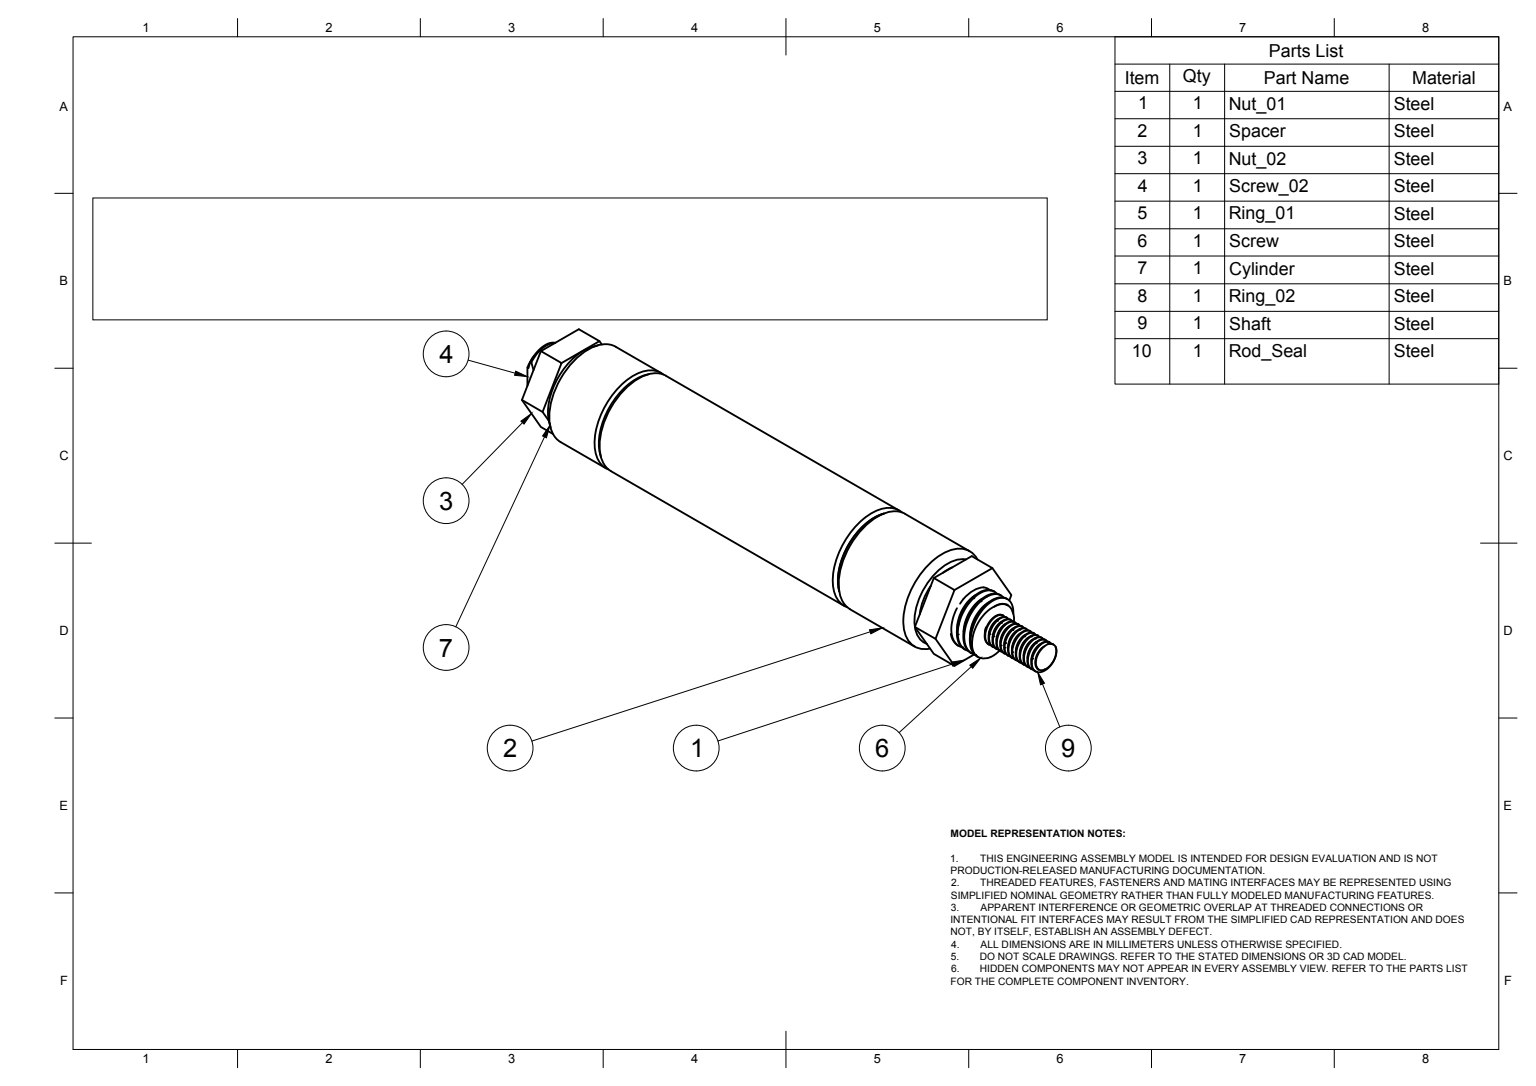
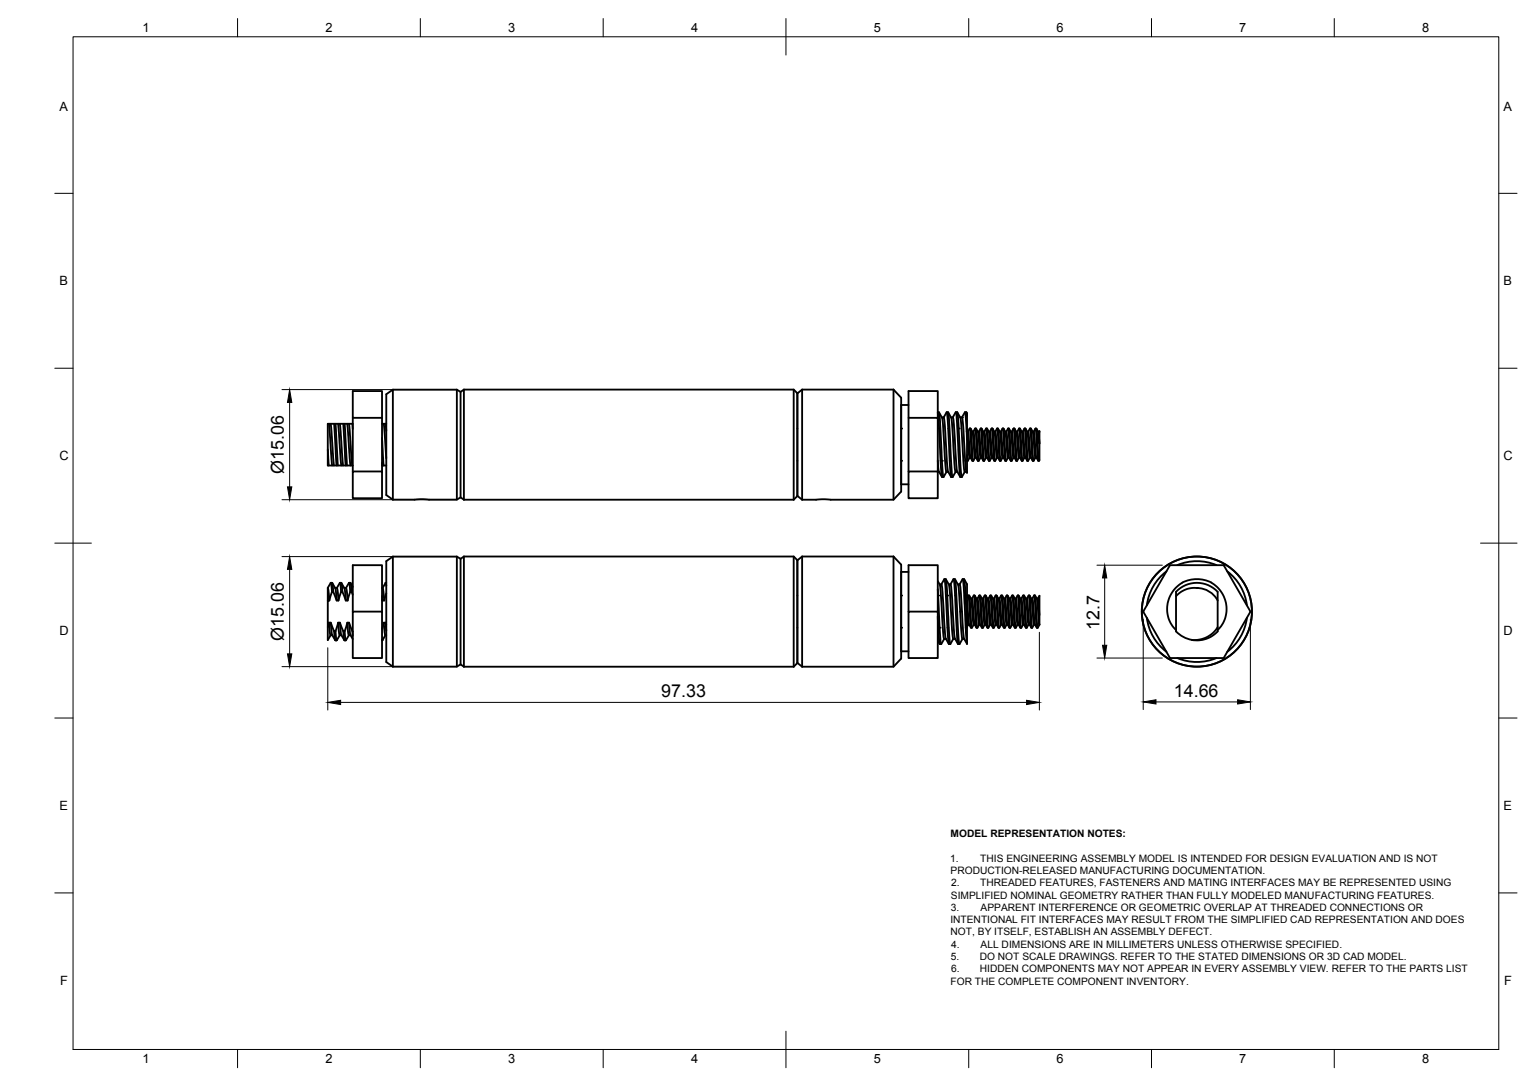
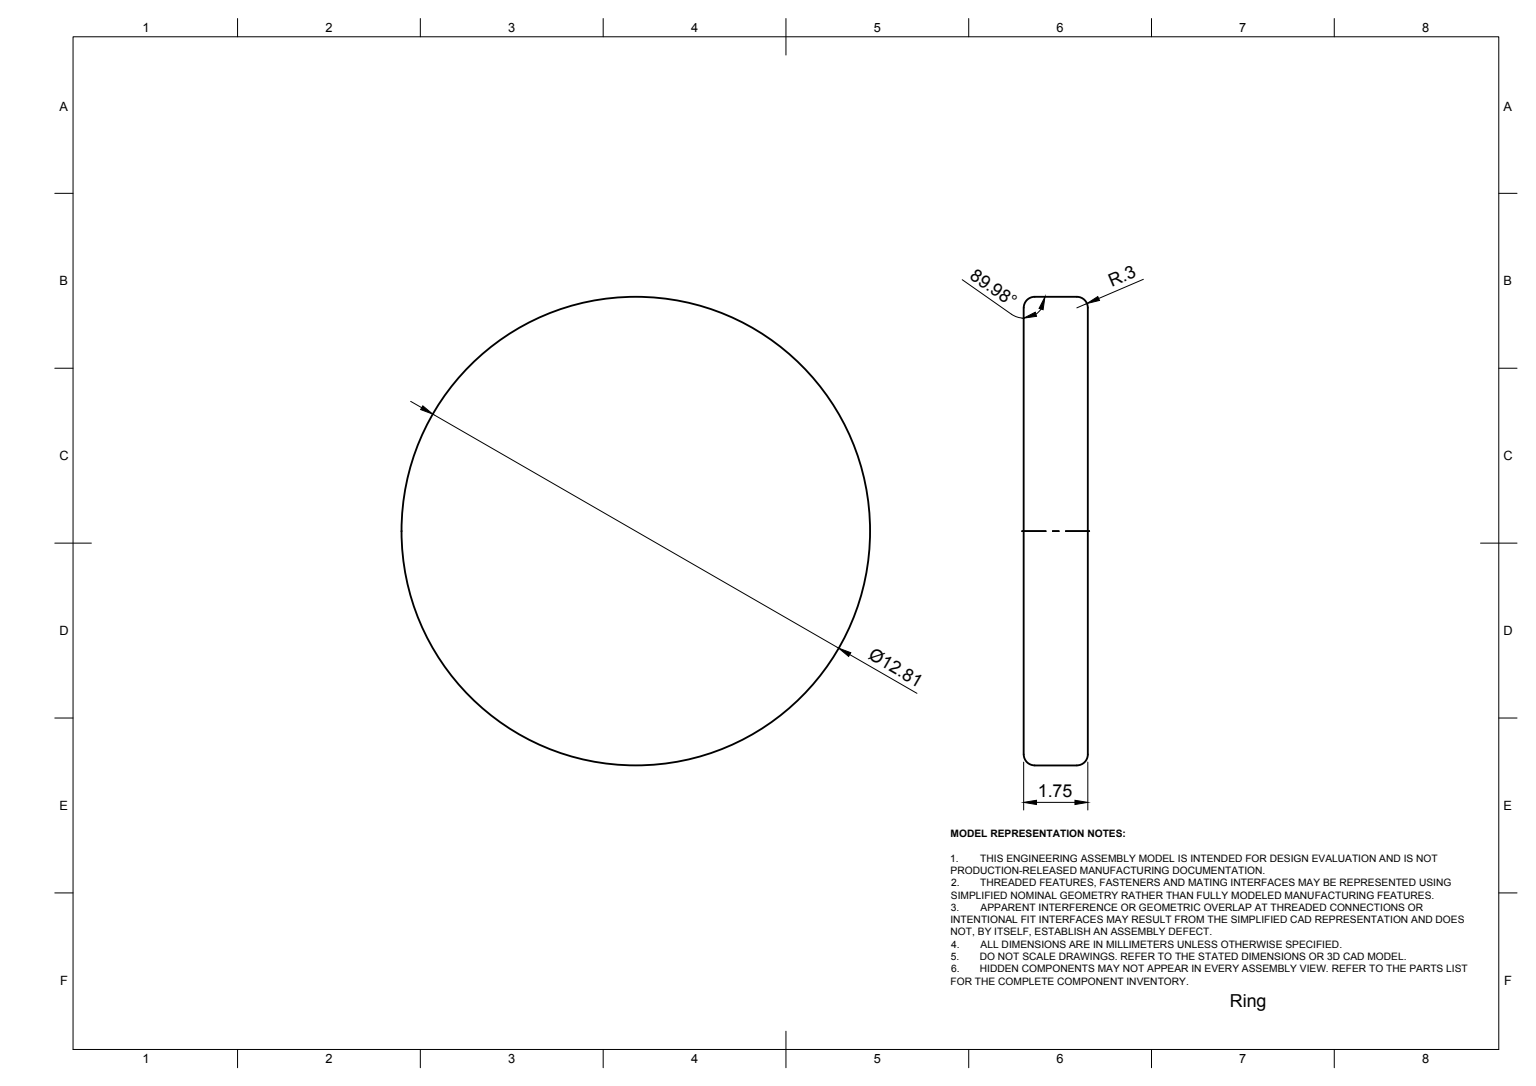
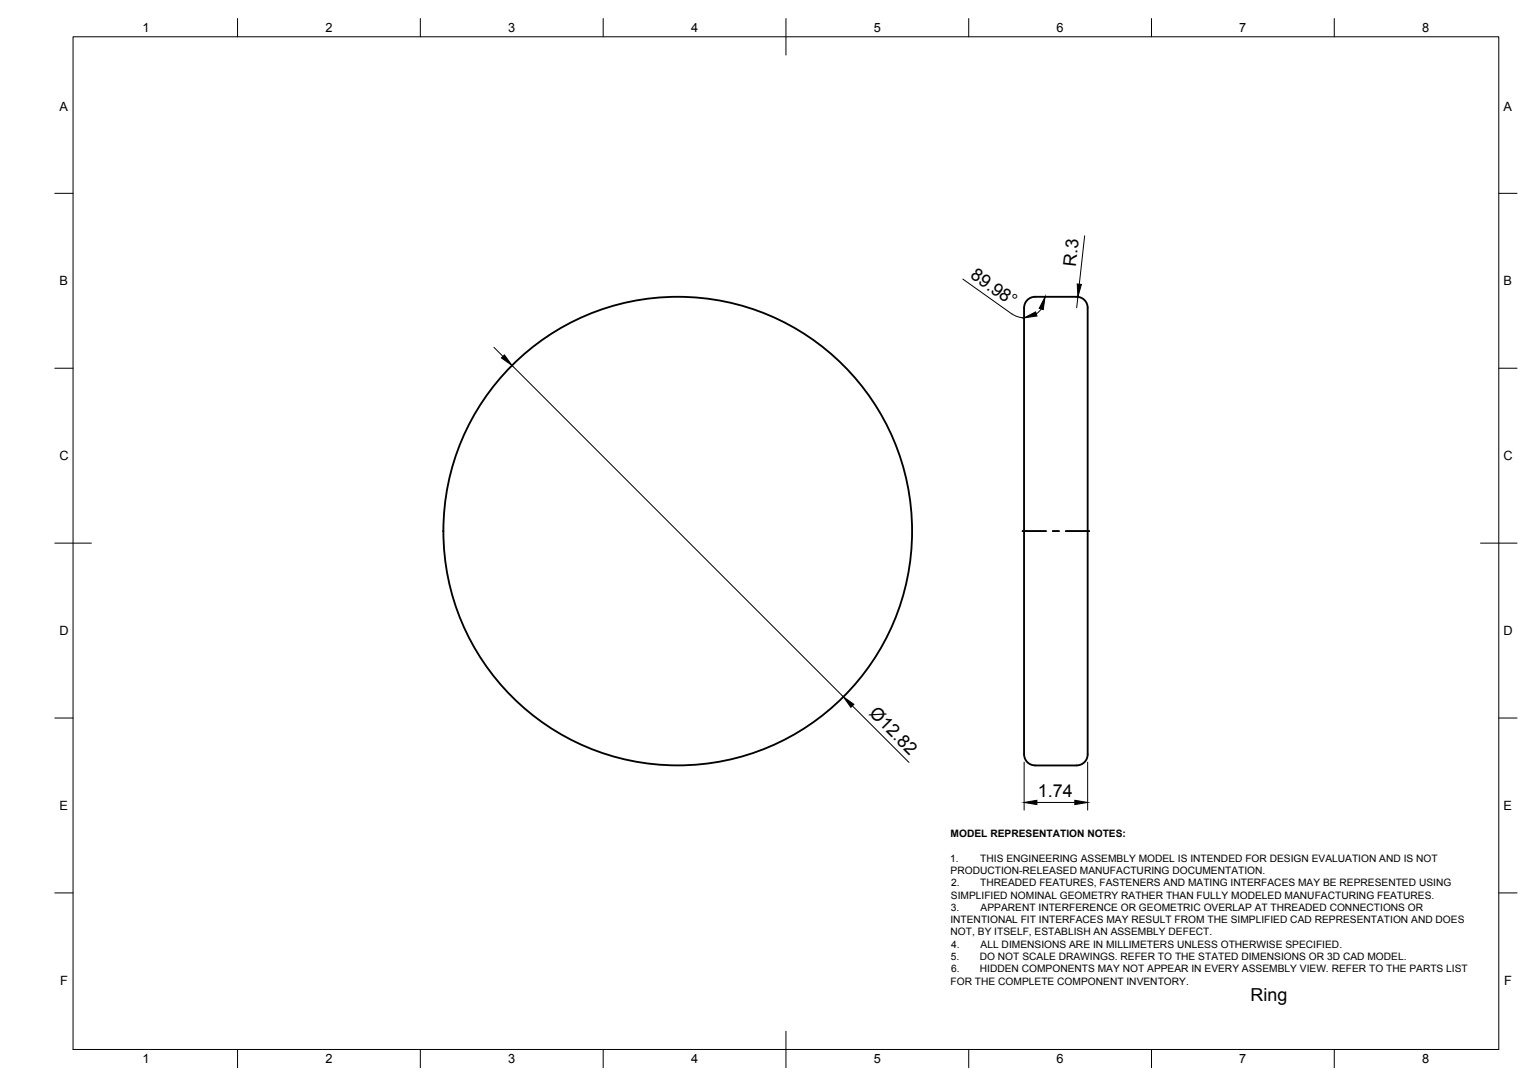
ISO-10303-21;
HEADER;
/* Generated by software containing ST-Developer
 * from STEP Tools, Inc. (www.steptools.com) 
 */

FILE_DESCRIPTION(
/* description */ (''),
/* implementation_level */ '2;1');

FILE_NAME(
/* name */ 'BR-314',
/* time_stamp */ '2026-10-06T13:15:55-07:00',
/* author */ (''),
/* organization */ (''),
/* preprocessor_version */ 'ST-DEVELOPER v20.2',
/* originating_system */ 'Autodesk Translation Framework v15.15.0.0',
/* authorisation */ '');

FILE_SCHEMA (('AUTOMOTIVE_DESIGN { 1 0 10303 214 3 1 1 }'));
ENDSEC;

DATA;
#10=MECHANICAL_DESIGN_GEOMETRIC_PRESENTATION_REPRESENTATION('',(#108,#109,
#110,#111,#112,#113,#114,#115,#116,#117),#27707);
#11=ITEM_DEFINED_TRANSFORMATION($,$,#3956,#4278);
#12=ITEM_DEFINED_TRANSFORMATION($,$,#3971,#4279);
#13=ITEM_DEFINED_TRANSFORMATION($,$,#3993,#4280);
#14=ITEM_DEFINED_TRANSFORMATION($,$,#4008,#4281);
#15=ITEM_DEFINED_TRANSFORMATION($,$,#4052,#4282);
#16=ITEM_DEFINED_TRANSFORMATION($,$,#4064,#4283);
#17=ITEM_DEFINED_TRANSFORMATION($,$,#4092,#4284);
#18=ITEM_DEFINED_TRANSFORMATION($,$,#4144,#4285);
#19=ITEM_DEFINED_TRANSFORMATION($,$,#4156,#4286);
#20=ITEM_DEFINED_TRANSFORMATION($,$,#4269,#4287);
#21=(
REPRESENTATION_RELATIONSHIP($,$,#27745,#27744)
REPRESENTATION_RELATIONSHIP_WITH_TRANSFORMATION(#11)
SHAPE_REPRESENTATION_RELATIONSHIP()
);
#22=(
REPRESENTATION_RELATIONSHIP($,$,#27746,#27744)
REPRESENTATION_RELATIONSHIP_WITH_TRANSFORMATION(#12)
SHAPE_REPRESENTATION_RELATIONSHIP()
);
#23=(
REPRESENTATION_RELATIONSHIP($,$,#27747,#27744)
REPRESENTATION_RELATIONSHIP_WITH_TRANSFORMATION(#13)
SHAPE_REPRESENTATION_RELATIONSHIP()
);
#24=(
REPRESENTATION_RELATIONSHIP($,$,#27748,#27744)
REPRESENTATION_RELATIONSHIP_WITH_TRANSFORMATION(#14)
SHAPE_REPRESENTATION_RELATIONSHIP()
);
#25=(
REPRESENTATION_RELATIONSHIP($,$,#27749,#27744)
REPRESENTATION_RELATIONSHIP_WITH_TRANSFORMATION(#15)
SHAPE_REPRESENTATION_RELATIONSHIP()
);
#26=(
REPRESENTATION_RELATIONSHIP($,$,#27750,#27744)
REPRESENTATION_RELATIONSHIP_WITH_TRANSFORMATION(#16)
SHAPE_REPRESENTATION_RELATIONSHIP()
);
#27=(
REPRESENTATION_RELATIONSHIP($,$,#27751,#27744)
REPRESENTATION_RELATIONSHIP_WITH_TRANSFORMATION(#17)
SHAPE_REPRESENTATION_RELATIONSHIP()
);
#28=(
REPRESENTATION_RELATIONSHIP($,$,#27752,#27744)
REPRESENTATION_RELATIONSHIP_WITH_TRANSFORMATION(#18)
SHAPE_REPRESENTATION_RELATIONSHIP()
);
#29=(
REPRESENTATION_RELATIONSHIP($,$,#27753,#27744)
REPRESENTATION_RELATIONSHIP_WITH_TRANSFORMATION(#19)
SHAPE_REPRESENTATION_RELATIONSHIP()
);
#30=(
REPRESENTATION_RELATIONSHIP($,$,#27754,#27744)
REPRESENTATION_RELATIONSHIP_WITH_TRANSFORMATION(#20)
SHAPE_REPRESENTATION_RELATIONSHIP()
);
#31=CONTEXT_DEPENDENT_SHAPE_REPRESENTATION(#21,#27734);
#32=CONTEXT_DEPENDENT_SHAPE_REPRESENTATION(#22,#27735);
#33=CONTEXT_DEPENDENT_SHAPE_REPRESENTATION(#23,#27736);
#34=CONTEXT_DEPENDENT_SHAPE_REPRESENTATION(#24,#27737);
#35=CONTEXT_DEPENDENT_SHAPE_REPRESENTATION(#25,#27738);
#36=CONTEXT_DEPENDENT_SHAPE_REPRESENTATION(#26,#27739);
#37=CONTEXT_DEPENDENT_SHAPE_REPRESENTATION(#27,#27740);
#38=CONTEXT_DEPENDENT_SHAPE_REPRESENTATION(#28,#27741);
#39=CONTEXT_DEPENDENT_SHAPE_REPRESENTATION(#29,#27742);
#40=CONTEXT_DEPENDENT_SHAPE_REPRESENTATION(#30,#27743);
#41=NEXT_ASSEMBLY_USAGE_OCCURRENCE('Nut_01:1','Nut_01:1','Nut_01:1',#27756,
#27757,'Nut_01:1');
#42=NEXT_ASSEMBLY_USAGE_OCCURRENCE('Spacer:1','Spacer:1','Spacer:1',#27756,
#27758,'Spacer:1');
#43=NEXT_ASSEMBLY_USAGE_OCCURRENCE('Nut_02:1','Nut_02:1','Nut_02:1',#27756,
#27759,'Nut_02:1');
#44=NEXT_ASSEMBLY_USAGE_OCCURRENCE('Screw_02:1','Screw_02:1',
'Screw_02:1',#27756,#27760,'Screw_02:1');
#45=NEXT_ASSEMBLY_USAGE_OCCURRENCE('Ring_01:1','Ring_01:1','Ring_01:1',
#27756,#27761,'Ring_01:1');
#46=NEXT_ASSEMBLY_USAGE_OCCURRENCE('Screw:1','Screw:1','Screw:1',#27756,
#27762,'Screw:1');
#47=NEXT_ASSEMBLY_USAGE_OCCURRENCE('Cylinder:1','Cylinder:1',
'Cylinder:1',#27756,#27763,'Cylinder:1');
#48=NEXT_ASSEMBLY_USAGE_OCCURRENCE('Ring_02:1','Ring_02:1','Ring_02:1',
#27756,#27764,'Ring_02:1');
#49=NEXT_ASSEMBLY_USAGE_OCCURRENCE('Shaft:1','Shaft:1','Shaft:1',#27756,
#27765,'Shaft:1');
#50=NEXT_ASSEMBLY_USAGE_OCCURRENCE('Rod_Seal:1','Rod_Seal:1',
'Rod_Seal:1',#27756,#27766,'Rod_Seal:1');
#51=TOROIDAL_SURFACE('',#4053,6.1074958342087,0.3);
#52=TOROIDAL_SURFACE('',#4060,6.1071549018742,0.3);
#53=TOROIDAL_SURFACE('',#4145,6.10923539706593,0.3);
#54=TOROIDAL_SURFACE('',#4152,6.1088989677085,0.3);
#55=TOROIDAL_SURFACE('',#4197,6.10845002480549,0.3);
#56=TOROIDAL_SURFACE('',#4203,6.107959450045,0.3);
#57=TOROIDAL_SURFACE('',#4209,4.18902817623056,0.3);
#58=TOROIDAL_SURFACE('',#4216,6.1096023907077,0.3);
#59=TOROIDAL_SURFACE('',#4223,6.10941276264524,0.3);
#60=TOROIDAL_SURFACE('',#4228,6.1087216021292,0.3);
#61=TOROIDAL_SURFACE('',#4236,6.1086273903848,0.3);
#62=TOROIDAL_SURFACE('',#4238,6.10778208446569,0.3);
#63=TOROIDAL_SURFACE('',#4243,6.10767319978801,0.3);
#64=TOROIDAL_SURFACE('',#4248,6.1069775362949,0.3);
#65=TOROIDAL_SURFACE('',#4256,6.10683442041659,0.3);
#66=TOROIDAL_SURFACE('',#4261,4.12329516333974,0.3);
#67=ELLIPSE('',#4027,3.36109563026061,2.90329889035631);
#68=ELLIPSE('',#4028,2.84121050972126,2.43735261139454);
#69=ELLIPSE('',#4046,3.33206993022602,2.82346550068506);
#70=CONICAL_SURFACE('',#3978,7.269,0.680431320864525);
#71=CONICAL_SURFACE('',#3982,6.974,0.81226843236958);
#72=CONICAL_SURFACE('',#4057,6.40732538114918,0.000295609290232334);
#73=CONICAL_SURFACE('',#4093,7.27835105742136,0.785398163397451);
#74=CONICAL_SURFACE('',#4106,7.20746054905241,0.610790367386849);
#75=CONICAL_SURFACE('',#4111,7.36529369971832,0.557210682142491);
#76=CONICAL_SURFACE('',#4113,7.36790580323689,0.610790367386849);
#77=CONICAL_SURFACE('',#4114,6.41628586403442,0.000295609290232646);
#78=CONICAL_SURFACE('',#4118,6.40906719549494,0.00029560929023293);
#79=CONICAL_SURFACE('',#4126,6.40820475053297,0.000295609290233083);
#80=CONICAL_SURFACE('',#4130,6.40732538114918,0.000295609290232334);
#81=CONICAL_SURFACE('',#4134,6.40667124022599,0.000295609290231853);
#82=CONICAL_SURFACE('',#4149,6.40906719549494,0.00029560929023293);
#83=CONICAL_SURFACE('',#4201,6.40820475053297,0.000295609290233083);
#84=CONICAL_SURFACE('',#4220,6.40950758978419,0.000295609290232241);
#85=CONICAL_SURFACE('',#4232,6.40867450936473,0.000295609290232273);
#86=CONICAL_SURFACE('',#4241,6.40772765523458,0.000295609290232245);
#87=CONICAL_SURFACE('',#4252,6.40690599146347,0.000295609290233429);
#88=SHAPE_REPRESENTATION_RELATIONSHIP('SRR','None',#27745,#98);
#89=SHAPE_REPRESENTATION_RELATIONSHIP('SRR','None',#27746,#99);
#90=SHAPE_REPRESENTATION_RELATIONSHIP('SRR','None',#27747,#100);
#91=SHAPE_REPRESENTATION_RELATIONSHIP('SRR','None',#27748,#101);
#92=SHAPE_REPRESENTATION_RELATIONSHIP('SRR','None',#27749,#102);
#93=SHAPE_REPRESENTATION_RELATIONSHIP('SRR','None',#27750,#103);
#94=SHAPE_REPRESENTATION_RELATIONSHIP('SRR','None',#27751,#104);
#95=SHAPE_REPRESENTATION_RELATIONSHIP('SRR','None',#27752,#105);
#96=SHAPE_REPRESENTATION_RELATIONSHIP('SRR','None',#27753,#106);
#97=SHAPE_REPRESENTATION_RELATIONSHIP('SRR','None',#27754,#107);
#98=ADVANCED_BREP_SHAPE_REPRESENTATION('',(#118),#27697);
#99=ADVANCED_BREP_SHAPE_REPRESENTATION('',(#119),#27698);
#100=ADVANCED_BREP_SHAPE_REPRESENTATION('',(#120),#27699);
#101=ADVANCED_BREP_SHAPE_REPRESENTATION('',(#121),#27700);
#102=ADVANCED_BREP_SHAPE_REPRESENTATION('',(#122),#27701);
#103=ADVANCED_BREP_SHAPE_REPRESENTATION('',(#123),#27702);
#104=ADVANCED_BREP_SHAPE_REPRESENTATION('',(#124),#27703);
#105=ADVANCED_BREP_SHAPE_REPRESENTATION('',(#125),#27704);
#106=ADVANCED_BREP_SHAPE_REPRESENTATION('',(#126),#27705);
#107=ADVANCED_BREP_SHAPE_REPRESENTATION('',(#127),#27706);
#108=STYLED_ITEM('',(#27804),#118);
#109=STYLED_ITEM('',(#27804),#119);
#110=STYLED_ITEM('',(#27804),#120);
#111=STYLED_ITEM('',(#27804),#121);
#112=STYLED_ITEM('',(#27804),#122);
#113=STYLED_ITEM('',(#27804),#123);
#114=STYLED_ITEM('',(#27804),#124);
#115=STYLED_ITEM('',(#27804),#125);
#116=STYLED_ITEM('',(#27804),#126);
#117=STYLED_ITEM('',(#27804),#127);
#118=MANIFOLD_SOLID_BREP('Body1',#3834);
#119=MANIFOLD_SOLID_BREP('Body1',#3835);
#120=MANIFOLD_SOLID_BREP('Body1',#3836);
#121=MANIFOLD_SOLID_BREP('Body1',#3837);
#122=MANIFOLD_SOLID_BREP('Body1',#3838);
#123=MANIFOLD_SOLID_BREP('Body1',#3839);
#124=MANIFOLD_SOLID_BREP('Body1',#3840);
#125=MANIFOLD_SOLID_BREP('Body1',#3841);
#126=MANIFOLD_SOLID_BREP('Body1',#3842);
#127=MANIFOLD_SOLID_BREP('Body1',#3843);
#128=FACE_BOUND('',#670,.T.);
#129=FACE_BOUND('',#672,.T.);
#130=FACE_BOUND('',#675,.T.);
#131=FACE_BOUND('',#677,.T.);
#132=FACE_BOUND('',#680,.T.);
#133=FACE_BOUND('',#683,.T.);
#134=FACE_BOUND('',#686,.T.);
#135=FACE_BOUND('',#689,.T.);
#136=FACE_BOUND('',#701,.T.);
#137=FACE_BOUND('',#703,.T.);
#138=FACE_BOUND('',#765,.T.);
#139=FACE_BOUND('',#789,.T.);
#140=FACE_BOUND('',#791,.T.);
#141=FACE_BOUND('',#793,.T.);
#142=FACE_BOUND('',#796,.T.);
#143=FACE_BOUND('',#801,.T.);
#144=FACE_BOUND('',#804,.T.);
#145=FACE_BOUND('',#811,.T.);
#146=FACE_BOUND('',#814,.T.);
#147=FACE_BOUND('',#821,.T.);
#148=FACE_BOUND('',#824,.T.);
#149=FACE_BOUND('',#826,.T.);
#150=FACE_BOUND('',#828,.T.);
#151=FACE_BOUND('',#835,.T.);
#152=FACE_BOUND('',#866,.T.);
#153=FACE_BOUND('',#871,.T.);
#154=FACE_BOUND('',#879,.T.);
#155=FACE_BOUND('',#883,.T.);
#156=FACE_BOUND('',#886,.T.);
#157=FACE_BOUND('',#890,.T.);
#158=FACE_BOUND('',#896,.T.);
#159=FACE_BOUND('',#900,.T.);
#160=FACE_BOUND('',#903,.T.);
#161=FACE_BOUND('',#911,.T.);
#162=FACE_BOUND('',#914,.T.);
#163=PLANE('',#3963);
#164=PLANE('',#3964);
#165=PLANE('',#3965);
#166=PLANE('',#3966);
#167=PLANE('',#3967);
#168=PLANE('',#3968);
#169=PLANE('',#3969);
#170=PLANE('',#3970);
#171=PLANE('',#3976);
#172=PLANE('',#3984);
#173=PLANE('',#3988);
#174=PLANE('',#3992);
#175=PLANE('',#4000);
#176=PLANE('',#4001);
#177=PLANE('',#4002);
#178=PLANE('',#4003);
#179=PLANE('',#4004);
#180=PLANE('',#4005);
#181=PLANE('',#4006);
#182=PLANE('',#4007);
#183=PLANE('',#4009);
#184=PLANE('',#4010);
#185=PLANE('',#4029);
#186=PLANE('',#4050);
#187=PLANE('',#4051);
#188=PLANE('',#4059);
#189=PLANE('',#4063);
#190=PLANE('',#4080);
#191=PLANE('',#4089);
#192=PLANE('',#4090);
#193=PLANE('',#4091);
#194=PLANE('',#4096);
#195=PLANE('',#4104);
#196=PLANE('',#4120);
#197=PLANE('',#4124);
#198=PLANE('',#4136);
#199=PLANE('',#4140);
#200=PLANE('',#4143);
#201=PLANE('',#4151);
#202=PLANE('',#4155);
#203=PLANE('',#4191);
#204=PLANE('',#4194);
#205=PLANE('',#4205);
#206=PLANE('',#4207);
#207=PLANE('',#4208);
#208=PLANE('',#4215);
#209=PLANE('',#4222);
#210=PLANE('',#4226);
#211=PLANE('',#4234);
#212=PLANE('',#4246);
#213=PLANE('',#4254);
#214=PLANE('',#4259);
#215=PLANE('',#4265);
#216=PLANE('',#4273);
#217=PLANE('',#4277);
#218=CIRCLE('',#3958,4.433);
#219=CIRCLE('',#3959,4.433);
#220=CIRCLE('',#3961,3.72275);
#221=CIRCLE('',#3962,3.72275);
#222=CIRCLE('',#3974,4.75);
#223=CIRCLE('',#3975,4.75);
#224=CIRCLE('',#3977,7.01);
#225=CIRCLE('',#3979,7.528);
#226=CIRCLE('',#3981,7.528);
#227=CIRCLE('',#3983,6.42);
#228=CIRCLE('',#3985,3.7);
#229=CIRCLE('',#3987,3.7);
#230=CIRCLE('',#3989,2.204);
#231=CIRCLE('',#3991,2.204);
#232=CIRCLE('',#3995,4.433);
#233=CIRCLE('',#3996,4.433);
#234=CIRCLE('',#3998,3.72275);
#235=CIRCLE('',#3999,3.72275);
#236=CIRCLE('',#4012,3.22275);
#237=CIRCLE('',#4026,3.22275);
#238=CIRCLE('',#4030,3.933);
#239=CIRCLE('',#4033,3.933);
#240=CIRCLE('',#4048,5.);
#241=CIRCLE('',#4049,5.);
#242=CIRCLE('',#4054,6.1074958342087);
#243=CIRCLE('',#4055,0.3);
#244=CIRCLE('',#4056,6.40749582110097);
#245=CIRCLE('',#4058,6.40715488876647);
#246=CIRCLE('',#4061,0.3);
#247=CIRCLE('',#4062,6.1071549018742);
#248=CIRCLE('',#4066,3.72275);
#249=CIRCLE('',#4073,3.72275);
#250=CIRCLE('',#4075,4.433);
#251=CIRCLE('',#4076,4.433);
#252=CIRCLE('',#4078,1.77625);
#253=CIRCLE('',#4079,1.77625);
#254=CIRCLE('',#4081,2.204);
#255=CIRCLE('',#4082,2.204);
#256=CIRCLE('',#4084,2.204);
#257=CIRCLE('',#4085,2.204);
#258=CIRCLE('',#4087,5.42440960677665);
#259=CIRCLE('',#4088,5.42440960677665);
#260=CIRCLE('',#4094,7.52835105742136);
#261=CIRCLE('',#4095,7.02835105742136);
#262=CIRCLE('',#4097,6.42021067919505);
#263=CIRCLE('',#4099,7.52835105742136);
#264=CIRCLE('',#4102,5.);
#265=CIRCLE('',#4103,5.);
#266=CIRCLE('',#4105,3.44589712386029);
#267=CIRCLE('',#4107,7.52312685038423);
#268=CIRCLE('',#4108,6.89179424772059);
#269=CIRCLE('',#4110,7.52312685038423);
#270=CIRCLE('',#4112,7.20746054905241);
#271=CIRCLE('',#4115,6.40969108660508);
#272=CIRCLE('',#4117,6.40969108660508);
#273=CIRCLE('',#4119,6.40881029802658);
#274=CIRCLE('',#4121,6.41550316824698);
#275=CIRCLE('',#4123,6.41550316824698);
#276=CIRCLE('',#4125,6.40853872070288);
#277=CIRCLE('',#4127,6.40787078036307);
#278=CIRCLE('',#4129,6.40787078036307);
#279=CIRCLE('',#4131,6.40706623219228);
#280=CIRCLE('',#4133,6.40706623219228);
#281=CIRCLE('',#4135,6.4065967297173);
#282=CIRCLE('',#4137,4.66385643997278);
#283=CIRCLE('',#4139,4.66385643997278);
#284=CIRCLE('',#4141,3.44589712386029);
#285=CIRCLE('',#4146,6.10923539706593);
#286=CIRCLE('',#4147,0.3);
#287=CIRCLE('',#4148,6.4092353839582);
#288=CIRCLE('',#4150,6.40889895460077);
#289=CIRCLE('',#4153,0.3);
#290=CIRCLE('',#4154,6.1088989677085);
#291=CIRCLE('',#4158,2.204);
#292=CIRCLE('',#4159,2.204);
#293=CIRCLE('',#4160,2.204);
#294=CIRCLE('',#4174,1.77625);
#295=CIRCLE('',#4188,1.77625);
#296=CIRCLE('',#4190,0.999999999999996);
#297=CIRCLE('',#4193,2.204);
#298=CIRCLE('',#4195,6.107959450045);
#299=CIRCLE('',#4196,6.10778208446569);
#300=CIRCLE('',#4198,6.10845002480549);
#301=CIRCLE('',#4199,0.3);
#302=CIRCLE('',#4200,6.40845001169777);
#303=CIRCLE('',#4202,6.40795943693727);
#304=CIRCLE('',#4204,0.3);
#305=CIRCLE('',#4206,6.1086273903848);
#306=CIRCLE('',#4210,4.18902817623056);
#307=CIRCLE('',#4211,0.3);
#308=CIRCLE('',#4212,4.48902817623056);
#309=CIRCLE('',#4214,4.48902817623056);
#310=CIRCLE('',#4217,6.1096023907077);
#311=CIRCLE('',#4218,0.3);
#312=CIRCLE('',#4219,6.40960237759997);
#313=CIRCLE('',#4221,6.40941274953751);
#314=CIRCLE('',#4224,0.3);
#315=CIRCLE('',#4225,6.10941276264524);
#316=CIRCLE('',#4227,2.21164758166987);
#317=CIRCLE('',#4229,6.1087216021292);
#318=CIRCLE('',#4230,0.3);
#319=CIRCLE('',#4231,6.40872158902147);
#320=CIRCLE('',#4233,6.40862737727707);
#321=CIRCLE('',#4235,2.21164758166987);
#322=CIRCLE('',#4237,0.3);
#323=CIRCLE('',#4239,0.3);
#324=CIRCLE('',#4240,6.40778207135796);
#325=CIRCLE('',#4242,6.40767318668028);
#326=CIRCLE('',#4244,0.3);
#327=CIRCLE('',#4245,6.10767319978801);
#328=CIRCLE('',#4247,2.21164758166987);
#329=CIRCLE('',#4249,6.1069775362949);
#330=CIRCLE('',#4250,0.3);
#331=CIRCLE('',#4251,6.40697752318717);
#332=CIRCLE('',#4253,6.40683440730886);
#333=CIRCLE('',#4255,2.21164758166987);
#334=CIRCLE('',#4257,0.3);
#335=CIRCLE('',#4258,6.10683442041659);
#336=CIRCLE('',#4260,4.42329516333974);
#337=CIRCLE('',#4262,4.42329516333974);
#338=CIRCLE('',#4263,0.3);
#339=CIRCLE('',#4264,4.12329516333974);
#340=CIRCLE('',#4271,3.7);
#341=CIRCLE('',#4272,3.7);
#342=CIRCLE('',#4274,2.204);
#343=CIRCLE('',#4276,2.204);
#344=CYLINDRICAL_SURFACE('',#3957,4.433);
#345=CYLINDRICAL_SURFACE('',#3960,3.72275);
#346=CYLINDRICAL_SURFACE('',#3972,0.999999999999996);
#347=CYLINDRICAL_SURFACE('',#3973,4.75);
#348=CYLINDRICAL_SURFACE('',#3980,7.528);
#349=CYLINDRICAL_SURFACE('',#3986,3.7);
#350=CYLINDRICAL_SURFACE('',#3990,2.204);
#351=CYLINDRICAL_SURFACE('',#3994,4.433);
#352=CYLINDRICAL_SURFACE('',#3997,3.72275);
#353=CYLINDRICAL_SURFACE('',#4011,3.22275);
#354=CYLINDRICAL_SURFACE('',#4013,3.22275);
#355=CYLINDRICAL_SURFACE('',#4014,3.22275);
#356=CYLINDRICAL_SURFACE('',#4015,3.22275);
#357=CYLINDRICAL_SURFACE('',#4016,3.22275);
#358=CYLINDRICAL_SURFACE('',#4017,3.22275);
#359=CYLINDRICAL_SURFACE('',#4018,3.22275);
#360=CYLINDRICAL_SURFACE('',#4019,3.22275);
#361=CYLINDRICAL_SURFACE('',#4020,3.22275);
#362=CYLINDRICAL_SURFACE('',#4021,3.22275);
#363=CYLINDRICAL_SURFACE('',#4022,3.22275);
#364=CYLINDRICAL_SURFACE('',#4023,3.22275);
#365=CYLINDRICAL_SURFACE('',#4024,3.22275);
#366=CYLINDRICAL_SURFACE('',#4025,3.22275);
#367=CYLINDRICAL_SURFACE('',#4031,3.933);
#368=CYLINDRICAL_SURFACE('',#4032,3.933);
#369=CYLINDRICAL_SURFACE('',#4034,3.933);
#370=CYLINDRICAL_SURFACE('',#4035,3.933);
#371=CYLINDRICAL_SURFACE('',#4036,3.933);
#372=CYLINDRICAL_SURFACE('',#4037,3.933);
#373=CYLINDRICAL_SURFACE('',#4038,3.933);
#374=CYLINDRICAL_SURFACE('',#4039,3.933);
#375=CYLINDRICAL_SURFACE('',#4040,3.933);
#376=CYLINDRICAL_SURFACE('',#4041,3.933);
#377=CYLINDRICAL_SURFACE('',#4042,3.933);
#378=CYLINDRICAL_SURFACE('',#4043,3.933);
#379=CYLINDRICAL_SURFACE('',#4044,3.933);
#380=CYLINDRICAL_SURFACE('',#4045,3.933);
#381=CYLINDRICAL_SURFACE('',#4047,5.);
#382=CYLINDRICAL_SURFACE('',#4065,3.72275);
#383=CYLINDRICAL_SURFACE('',#4067,3.72275);
#384=CYLINDRICAL_SURFACE('',#4068,3.72275);
#385=CYLINDRICAL_SURFACE('',#4069,3.72275);
#386=CYLINDRICAL_SURFACE('',#4070,3.72275);
#387=CYLINDRICAL_SURFACE('',#4071,3.72275);
#388=CYLINDRICAL_SURFACE('',#4072,3.72275);
#389=CYLINDRICAL_SURFACE('',#4074,4.433);
#390=CYLINDRICAL_SURFACE('',#4077,1.77625);
#391=CYLINDRICAL_SURFACE('',#4083,2.204);
#392=CYLINDRICAL_SURFACE('',#4086,5.42440960677665);
#393=CYLINDRICAL_SURFACE('',#4098,7.52835105742136);
#394=CYLINDRICAL_SURFACE('',#4100,0.999999999999999);
#395=CYLINDRICAL_SURFACE('',#4101,5.);
#396=CYLINDRICAL_SURFACE('',#4109,7.52312685038423);
#397=CYLINDRICAL_SURFACE('',#4116,6.40969108660508);
#398=CYLINDRICAL_SURFACE('',#4122,6.41550316824698);
#399=CYLINDRICAL_SURFACE('',#4128,6.40787078036307);
#400=CYLINDRICAL_SURFACE('',#4132,6.40706623219228);
#401=CYLINDRICAL_SURFACE('',#4138,4.66385643997278);
#402=CYLINDRICAL_SURFACE('',#4142,3.44589712386029);
#403=CYLINDRICAL_SURFACE('',#4157,2.204);
#404=CYLINDRICAL_SURFACE('',#4161,2.204);
#405=CYLINDRICAL_SURFACE('',#4162,2.204);
#406=CYLINDRICAL_SURFACE('',#4163,2.204);
#407=CYLINDRICAL_SURFACE('',#4164,2.204);
#408=CYLINDRICAL_SURFACE('',#4165,2.204);
#409=CYLINDRICAL_SURFACE('',#4166,2.204);
#410=CYLINDRICAL_SURFACE('',#4167,2.204);
#411=CYLINDRICAL_SURFACE('',#4168,2.204);
#412=CYLINDRICAL_SURFACE('',#4169,2.204);
#413=CYLINDRICAL_SURFACE('',#4170,2.204);
#414=CYLINDRICAL_SURFACE('',#4171,2.204);
#415=CYLINDRICAL_SURFACE('',#4172,2.204);
#416=CYLINDRICAL_SURFACE('',#4173,1.77625);
#417=CYLINDRICAL_SURFACE('',#4175,1.77625);
#418=CYLINDRICAL_SURFACE('',#4176,1.77625);
#419=CYLINDRICAL_SURFACE('',#4177,1.77625);
#420=CYLINDRICAL_SURFACE('',#4178,1.77625);
#421=CYLINDRICAL_SURFACE('',#4179,1.77625);
#422=CYLINDRICAL_SURFACE('',#4180,1.77625);
#423=CYLINDRICAL_SURFACE('',#4181,1.77625);
#424=CYLINDRICAL_SURFACE('',#4182,1.77625);
#425=CYLINDRICAL_SURFACE('',#4183,1.77625);
#426=CYLINDRICAL_SURFACE('',#4184,1.77625);
#427=CYLINDRICAL_SURFACE('',#4185,1.77625);
#428=CYLINDRICAL_SURFACE('',#4186,1.77625);
#429=CYLINDRICAL_SURFACE('',#4187,1.77625);
#430=CYLINDRICAL_SURFACE('',#4189,0.999999999999996);
#431=CYLINDRICAL_SURFACE('',#4192,2.204);
#432=CYLINDRICAL_SURFACE('',#4213,4.48902817623056);
#433=CYLINDRICAL_SURFACE('',#4266,4.42329516333974);
#434=CYLINDRICAL_SURFACE('',#4267,2.21164758166987);
#435=CYLINDRICAL_SURFACE('',#4268,2.21164758166987);
#436=CYLINDRICAL_SURFACE('',#4270,3.7);
#437=CYLINDRICAL_SURFACE('',#4275,2.204);
#438=FACE_OUTER_BOUND('',#659,.T.);
#439=FACE_OUTER_BOUND('',#660,.T.);
#440=FACE_OUTER_BOUND('',#661,.T.);
#441=FACE_OUTER_BOUND('',#662,.T.);
#442=FACE_OUTER_BOUND('',#663,.T.);
#443=FACE_OUTER_BOUND('',#664,.T.);
#444=FACE_OUTER_BOUND('',#665,.T.);
#445=FACE_OUTER_BOUND('',#666,.T.);
#446=FACE_OUTER_BOUND('',#667,.T.);
#447=FACE_OUTER_BOUND('',#668,.T.);
#448=FACE_OUTER_BOUND('',#669,.T.);
#449=FACE_OUTER_BOUND('',#671,.T.);
#450=FACE_OUTER_BOUND('',#673,.T.);
#451=FACE_OUTER_BOUND('',#674,.T.);
#452=FACE_OUTER_BOUND('',#676,.T.);
#453=FACE_OUTER_BOUND('',#678,.T.);
#454=FACE_OUTER_BOUND('',#679,.T.);
#455=FACE_OUTER_BOUND('',#681,.T.);
#456=FACE_OUTER_BOUND('',#682,.T.);
#457=FACE_OUTER_BOUND('',#684,.T.);
#458=FACE_OUTER_BOUND('',#685,.T.);
#459=FACE_OUTER_BOUND('',#687,.T.);
#460=FACE_OUTER_BOUND('',#688,.T.);
#461=FACE_OUTER_BOUND('',#690,.T.);
#462=FACE_OUTER_BOUND('',#691,.T.);
#463=FACE_OUTER_BOUND('',#692,.T.);
#464=FACE_OUTER_BOUND('',#693,.T.);
#465=FACE_OUTER_BOUND('',#694,.T.);
#466=FACE_OUTER_BOUND('',#695,.T.);
#467=FACE_OUTER_BOUND('',#696,.T.);
#468=FACE_OUTER_BOUND('',#697,.T.);
#469=FACE_OUTER_BOUND('',#698,.T.);
#470=FACE_OUTER_BOUND('',#699,.T.);
#471=FACE_OUTER_BOUND('',#700,.T.);
#472=FACE_OUTER_BOUND('',#702,.T.);
#473=FACE_OUTER_BOUND('',#704,.T.);
#474=FACE_OUTER_BOUND('',#705,.T.);
#475=FACE_OUTER_BOUND('',#706,.T.);
#476=FACE_OUTER_BOUND('',#707,.T.);
#477=FACE_OUTER_BOUND('',#708,.T.);
#478=FACE_OUTER_BOUND('',#709,.T.);
#479=FACE_OUTER_BOUND('',#710,.T.);
#480=FACE_OUTER_BOUND('',#711,.T.);
#481=FACE_OUTER_BOUND('',#712,.T.);
#482=FACE_OUTER_BOUND('',#713,.T.);
#483=FACE_OUTER_BOUND('',#714,.T.);
#484=FACE_OUTER_BOUND('',#715,.T.);
#485=FACE_OUTER_BOUND('',#716,.T.);
#486=FACE_OUTER_BOUND('',#717,.T.);
#487=FACE_OUTER_BOUND('',#718,.T.);
#488=FACE_OUTER_BOUND('',#719,.T.);
#489=FACE_OUTER_BOUND('',#720,.T.);
#490=FACE_OUTER_BOUND('',#721,.T.);
#491=FACE_OUTER_BOUND('',#722,.T.);
#492=FACE_OUTER_BOUND('',#723,.T.);
#493=FACE_OUTER_BOUND('',#724,.T.);
#494=FACE_OUTER_BOUND('',#725,.T.);
#495=FACE_OUTER_BOUND('',#726,.T.);
#496=FACE_OUTER_BOUND('',#727,.T.);
#497=FACE_OUTER_BOUND('',#728,.T.);
#498=FACE_OUTER_BOUND('',#729,.T.);
#499=FACE_OUTER_BOUND('',#730,.T.);
#500=FACE_OUTER_BOUND('',#731,.T.);
#501=FACE_OUTER_BOUND('',#732,.T.);
#502=FACE_OUTER_BOUND('',#733,.T.);
#503=FACE_OUTER_BOUND('',#734,.T.);
#504=FACE_OUTER_BOUND('',#735,.T.);
#505=FACE_OUTER_BOUND('',#736,.T.);
#506=FACE_OUTER_BOUND('',#737,.T.);
#507=FACE_OUTER_BOUND('',#738,.T.);
#508=FACE_OUTER_BOUND('',#739,.T.);
#509=FACE_OUTER_BOUND('',#740,.T.);
#510=FACE_OUTER_BOUND('',#741,.T.);
#511=FACE_OUTER_BOUND('',#742,.T.);
#512=FACE_OUTER_BOUND('',#743,.T.);
#513=FACE_OUTER_BOUND('',#744,.T.);
#514=FACE_OUTER_BOUND('',#745,.T.);
#515=FACE_OUTER_BOUND('',#746,.T.);
#516=FACE_OUTER_BOUND('',#747,.T.);
#517=FACE_OUTER_BOUND('',#748,.T.);
#518=FACE_OUTER_BOUND('',#749,.T.);
#519=FACE_OUTER_BOUND('',#750,.T.);
#520=FACE_OUTER_BOUND('',#751,.T.);
#521=FACE_OUTER_BOUND('',#752,.T.);
#522=FACE_OUTER_BOUND('',#753,.T.);
#523=FACE_OUTER_BOUND('',#754,.T.);
#524=FACE_OUTER_BOUND('',#755,.T.);
#525=FACE_OUTER_BOUND('',#756,.T.);
#526=FACE_OUTER_BOUND('',#757,.T.);
#527=FACE_OUTER_BOUND('',#758,.T.);
#528=FACE_OUTER_BOUND('',#759,.T.);
#529=FACE_OUTER_BOUND('',#760,.T.);
#530=FACE_OUTER_BOUND('',#761,.T.);
#531=FACE_OUTER_BOUND('',#762,.T.);
#532=FACE_OUTER_BOUND('',#763,.T.);
#533=FACE_OUTER_BOUND('',#764,.T.);
#534=FACE_OUTER_BOUND('',#766,.T.);
#535=FACE_OUTER_BOUND('',#767,.T.);
#536=FACE_OUTER_BOUND('',#768,.T.);
#537=FACE_OUTER_BOUND('',#769,.T.);
#538=FACE_OUTER_BOUND('',#770,.T.);
#539=FACE_OUTER_BOUND('',#771,.T.);
#540=FACE_OUTER_BOUND('',#772,.T.);
#541=FACE_OUTER_BOUND('',#773,.T.);
#542=FACE_OUTER_BOUND('',#774,.T.);
#543=FACE_OUTER_BOUND('',#775,.T.);
#544=FACE_OUTER_BOUND('',#776,.T.);
#545=FACE_OUTER_BOUND('',#777,.T.);
#546=FACE_OUTER_BOUND('',#778,.T.);
#547=FACE_OUTER_BOUND('',#779,.T.);
#548=FACE_OUTER_BOUND('',#780,.T.);
#549=FACE_OUTER_BOUND('',#781,.T.);
#550=FACE_OUTER_BOUND('',#782,.T.);
#551=FACE_OUTER_BOUND('',#783,.T.);
#552=FACE_OUTER_BOUND('',#784,.T.);
#553=FACE_OUTER_BOUND('',#785,.T.);
#554=FACE_OUTER_BOUND('',#786,.T.);
#555=FACE_OUTER_BOUND('',#787,.T.);
#556=FACE_OUTER_BOUND('',#788,.T.);
#557=FACE_OUTER_BOUND('',#790,.T.);
#558=FACE_OUTER_BOUND('',#792,.T.);
#559=FACE_OUTER_BOUND('',#794,.T.);
#560=FACE_OUTER_BOUND('',#795,.T.);
#561=FACE_OUTER_BOUND('',#797,.T.);
#562=FACE_OUTER_BOUND('',#798,.T.);
#563=FACE_OUTER_BOUND('',#799,.T.);
#564=FACE_OUTER_BOUND('',#800,.T.);
#565=FACE_OUTER_BOUND('',#802,.T.);
#566=FACE_OUTER_BOUND('',#803,.T.);
#567=FACE_OUTER_BOUND('',#805,.T.);
#568=FACE_OUTER_BOUND('',#806,.T.);
#569=FACE_OUTER_BOUND('',#807,.T.);
#570=FACE_OUTER_BOUND('',#808,.T.);
#571=FACE_OUTER_BOUND('',#809,.T.);
#572=FACE_OUTER_BOUND('',#810,.T.);
#573=FACE_OUTER_BOUND('',#812,.T.);
#574=FACE_OUTER_BOUND('',#813,.T.);
#575=FACE_OUTER_BOUND('',#815,.T.);
#576=FACE_OUTER_BOUND('',#816,.T.);
#577=FACE_OUTER_BOUND('',#817,.T.);
#578=FACE_OUTER_BOUND('',#818,.T.);
#579=FACE_OUTER_BOUND('',#819,.T.);
#580=FACE_OUTER_BOUND('',#820,.T.);
#581=FACE_OUTER_BOUND('',#822,.T.);
#582=FACE_OUTER_BOUND('',#823,.T.);
#583=FACE_OUTER_BOUND('',#825,.T.);
#584=FACE_OUTER_BOUND('',#827,.T.);
#585=FACE_OUTER_BOUND('',#829,.T.);
#586=FACE_OUTER_BOUND('',#830,.T.);
#587=FACE_OUTER_BOUND('',#831,.T.);
#588=FACE_OUTER_BOUND('',#832,.T.);
#589=FACE_OUTER_BOUND('',#833,.T.);
#590=FACE_OUTER_BOUND('',#834,.T.);
#591=FACE_OUTER_BOUND('',#836,.T.);
#592=FACE_OUTER_BOUND('',#837,.T.);
#593=FACE_OUTER_BOUND('',#838,.T.);
#594=FACE_OUTER_BOUND('',#839,.T.);
#595=FACE_OUTER_BOUND('',#840,.T.);
#596=FACE_OUTER_BOUND('',#841,.T.);
#597=FACE_OUTER_BOUND('',#842,.T.);
#598=FACE_OUTER_BOUND('',#843,.T.);
#599=FACE_OUTER_BOUND('',#844,.T.);
#600=FACE_OUTER_BOUND('',#845,.T.);
#601=FACE_OUTER_BOUND('',#846,.T.);
#602=FACE_OUTER_BOUND('',#847,.T.);
#603=FACE_OUTER_BOUND('',#848,.T.);
#604=FACE_OUTER_BOUND('',#849,.T.);
#605=FACE_OUTER_BOUND('',#850,.T.);
#606=FACE_OUTER_BOUND('',#851,.T.);
#607=FACE_OUTER_BOUND('',#852,.T.);
#608=FACE_OUTER_BOUND('',#853,.T.);
#609=FACE_OUTER_BOUND('',#854,.T.);
#610=FACE_OUTER_BOUND('',#855,.T.);
#611=FACE_OUTER_BOUND('',#856,.T.);
#612=FACE_OUTER_BOUND('',#857,.T.);
#613=FACE_OUTER_BOUND('',#858,.T.);
#614=FACE_OUTER_BOUND('',#859,.T.);
#615=FACE_OUTER_BOUND('',#860,.T.);
#616=FACE_OUTER_BOUND('',#861,.T.);
#617=FACE_OUTER_BOUND('',#862,.T.);
#618=FACE_OUTER_BOUND('',#863,.T.);
#619=FACE_OUTER_BOUND('',#864,.T.);
#620=FACE_OUTER_BOUND('',#865,.T.);
#621=FACE_OUTER_BOUND('',#867,.T.);
#622=FACE_OUTER_BOUND('',#868,.T.);
#623=FACE_OUTER_BOUND('',#869,.T.);
#624=FACE_OUTER_BOUND('',#870,.T.);
#625=FACE_OUTER_BOUND('',#872,.T.);
#626=FACE_OUTER_BOUND('',#873,.T.);
#627=FACE_OUTER_BOUND('',#874,.T.);
#628=FACE_OUTER_BOUND('',#875,.T.);
#629=FACE_OUTER_BOUND('',#876,.T.);
#630=FACE_OUTER_BOUND('',#877,.T.);
#631=FACE_OUTER_BOUND('',#878,.T.);
#632=FACE_OUTER_BOUND('',#880,.T.);
#633=FACE_OUTER_BOUND('',#881,.T.);
#634=FACE_OUTER_BOUND('',#882,.T.);
#635=FACE_OUTER_BOUND('',#884,.T.);
#636=FACE_OUTER_BOUND('',#885,.T.);
#637=FACE_OUTER_BOUND('',#887,.T.);
#638=FACE_OUTER_BOUND('',#888,.T.);
#639=FACE_OUTER_BOUND('',#889,.T.);
#640=FACE_OUTER_BOUND('',#891,.T.);
#641=FACE_OUTER_BOUND('',#892,.T.);
#642=FACE_OUTER_BOUND('',#893,.T.);
#643=FACE_OUTER_BOUND('',#894,.T.);
#644=FACE_OUTER_BOUND('',#895,.T.);
#645=FACE_OUTER_BOUND('',#897,.T.);
#646=FACE_OUTER_BOUND('',#898,.T.);
#647=FACE_OUTER_BOUND('',#899,.T.);
#648=FACE_OUTER_BOUND('',#901,.T.);
#649=FACE_OUTER_BOUND('',#902,.T.);
#650=FACE_OUTER_BOUND('',#904,.T.);
#651=FACE_OUTER_BOUND('',#905,.T.);
#652=FACE_OUTER_BOUND('',#906,.T.);
#653=FACE_OUTER_BOUND('',#907,.T.);
#654=FACE_OUTER_BOUND('',#908,.T.);
#655=FACE_OUTER_BOUND('',#909,.T.);
#656=FACE_OUTER_BOUND('',#910,.T.);
#657=FACE_OUTER_BOUND('',#912,.T.);
#658=FACE_OUTER_BOUND('',#913,.T.);
#659=EDGE_LOOP('',(#2457,#2458,#2459,#2460));
#660=EDGE_LOOP('',(#2461,#2462,#2463,#2464));
#661=EDGE_LOOP('',(#2465,#2466,#2467,#2468));
#662=EDGE_LOOP('',(#2469,#2470,#2471,#2472));
#663=EDGE_LOOP('',(#2473,#2474,#2475,#2476));
#664=EDGE_LOOP('',(#2477,#2478,#2479,#2480));
#665=EDGE_LOOP('',(#2481,#2482,#2483,#2484));
#666=EDGE_LOOP('',(#2485,#2486,#2487,#2488));
#667=EDGE_LOOP('',(#2489,#2490,#2491,#2492));
#668=EDGE_LOOP('',(#2493,#2494,#2495,#2496));
#669=EDGE_LOOP('',(#2497,#2498,#2499,#2500,#2501,#2502));
#670=EDGE_LOOP('',(#2503,#2504,#2505,#2506));
#671=EDGE_LOOP('',(#2507,#2508,#2509,#2510,#2511,#2512));
#672=EDGE_LOOP('',(#2513,#2514,#2515,#2516));
#673=EDGE_LOOP('',(#2517,#2518,#2519,#2520,#2521,#2522));
#674=EDGE_LOOP('',(#2523,#2524,#2525,#2526));
#675=EDGE_LOOP('',(#2527,#2528));
#676=EDGE_LOOP('',(#2529));
#677=EDGE_LOOP('',(#2530));
#678=EDGE_LOOP('',(#2531,#2532,#2533,#2534));
#679=EDGE_LOOP('',(#2535,#2536,#2537,#2538));
#680=EDGE_LOOP('',(#2539,#2540));
#681=EDGE_LOOP('',(#2541,#2542,#2543,#2544));
#682=EDGE_LOOP('',(#2545));
#683=EDGE_LOOP('',(#2546));
#684=EDGE_LOOP('',(#2547,#2548,#2549,#2550));
#685=EDGE_LOOP('',(#2551));
#686=EDGE_LOOP('',(#2552));
#687=EDGE_LOOP('',(#2553,#2554,#2555,#2556));
#688=EDGE_LOOP('',(#2557));
#689=EDGE_LOOP('',(#2558));
#690=EDGE_LOOP('',(#2559,#2560,#2561,#2562));
#691=EDGE_LOOP('',(#2563,#2564,#2565,#2566));
#692=EDGE_LOOP('',(#2567,#2568,#2569,#2570));
#693=EDGE_LOOP('',(#2571,#2572,#2573,#2574));
#694=EDGE_LOOP('',(#2575,#2576,#2577,#2578));
#695=EDGE_LOOP('',(#2579,#2580,#2581,#2582));
#696=EDGE_LOOP('',(#2583,#2584,#2585,#2586));
#697=EDGE_LOOP('',(#2587,#2588,#2589,#2590));
#698=EDGE_LOOP('',(#2591,#2592,#2593,#2594));
#699=EDGE_LOOP('',(#2595,#2596,#2597,#2598));
#700=EDGE_LOOP('',(#2599,#2600,#2601,#2602,#2603,#2604));
#701=EDGE_LOOP('',(#2605,#2606,#2607,#2608));
#702=EDGE_LOOP('',(#2609,#2610,#2611,#2612,#2613,#2614));
#703=EDGE_LOOP('',(#2615,#2616,#2617,#2618));
#704=EDGE_LOOP('',(#2619,#2620,#2621,#2622,#2623,#2624,#2625,#2626,#2627,
#2628,#2629,#2630,#2631,#2632,#2633,#2634,#2635,#2636,#2637,#2638,#2639,
#2640,#2641,#2642,#2643,#2644,#2645,#2646,#2647,#2648,#2649,#2650,#2651,
#2652,#2653,#2654,#2655,#2656,#2657,#2658,#2659,#2660,#2661,#2662,#2663,
#2664,#2665,#2666,#2667,#2668,#2669,#2670,#2671,#2672,#2673));
#705=EDGE_LOOP('',(#2674,#2675,#2676,#2677,#2678,#2679,#2680,#2681,#2682,
#2683,#2684,#2685,#2686,#2687,#2688,#2689,#2690,#2691,#2692,#2693,#2694,
#2695,#2696,#2697,#2698,#2699,#2700,#2701,#2702,#2703,#2704,#2705,#2706,
#2707,#2708,#2709,#2710,#2711,#2712,#2713,#2714,#2715,#2716,#2717,#2718,
#2719,#2720,#2721,#2722,#2723,#2724,#2725,#2726,#2727,#2728));
#706=EDGE_LOOP('',(#2729,#2730,#2731));
#707=EDGE_LOOP('',(#2732,#2733,#2734,#2735));
#708=EDGE_LOOP('',(#2736,#2737,#2738,#2739));
#709=EDGE_LOOP('',(#2740,#2741,#2742,#2743));
#710=EDGE_LOOP('',(#2744,#2745,#2746,#2747));
#711=EDGE_LOOP('',(#2748,#2749,#2750,#2751));
#712=EDGE_LOOP('',(#2752,#2753,#2754,#2755));
#713=EDGE_LOOP('',(#2756,#2757,#2758,#2759));
#714=EDGE_LOOP('',(#2760,#2761,#2762,#2763));
#715=EDGE_LOOP('',(#2764,#2765,#2766,#2767));
#716=EDGE_LOOP('',(#2768,#2769,#2770,#2771));
#717=EDGE_LOOP('',(#2772,#2773,#2774,#2775));
#718=EDGE_LOOP('',(#2776,#2777,#2778,#2779));
#719=EDGE_LOOP('',(#2780,#2781,#2782,#2783));
#720=EDGE_LOOP('',(#2784,#2785,#2786));
#721=EDGE_LOOP('',(#2787,#2788,#2789,#2790,#2791));
#722=EDGE_LOOP('',(#2792,#2793,#2794,#2795));
#723=EDGE_LOOP('',(#2796,#2797,#2798,#2799));
#724=EDGE_LOOP('',(#2800,#2801,#2802,#2803));
#725=EDGE_LOOP('',(#2804,#2805,#2806,#2807));
#726=EDGE_LOOP('',(#2808,#2809,#2810,#2811));
#727=EDGE_LOOP('',(#2812,#2813,#2814,#2815,#2816));
#728=EDGE_LOOP('',(#2817,#2818,#2819,#2820));
#729=EDGE_LOOP('',(#2821,#2822,#2823,#2824));
#730=EDGE_LOOP('',(#2825,#2826,#2827,#2828));
#731=EDGE_LOOP('',(#2829,#2830,#2831,#2832));
#732=EDGE_LOOP('',(#2833,#2834,#2835,#2836));
#733=EDGE_LOOP('',(#2837,#2838,#2839,#2840));
#734=EDGE_LOOP('',(#2841,#2842,#2843,#2844,#2845,#2846));
#735=EDGE_LOOP('',(#2847,#2848,#2849));
#736=EDGE_LOOP('',(#2850,#2851,#2852,#2853));
#737=EDGE_LOOP('',(#2854,#2855,#2856,#2857));
#738=EDGE_LOOP('',(#2858,#2859,#2860,#2861));
#739=EDGE_LOOP('',(#2862,#2863,#2864,#2865));
#740=EDGE_LOOP('',(#2866,#2867,#2868,#2869));
#741=EDGE_LOOP('',(#2870,#2871,#2872,#2873));
#742=EDGE_LOOP('',(#2874,#2875,#2876,#2877));
#743=EDGE_LOOP('',(#2878,#2879,#2880,#2881));
#744=EDGE_LOOP('',(#2882,#2883,#2884,#2885));
#745=EDGE_LOOP('',(#2886,#2887,#2888,#2889));
#746=EDGE_LOOP('',(#2890,#2891,#2892,#2893));
#747=EDGE_LOOP('',(#2894,#2895,#2896,#2897));
#748=EDGE_LOOP('',(#2898,#2899,#2900,#2901));
#749=EDGE_LOOP('',(#2902,#2903,#2904,#2905));
#750=EDGE_LOOP('',(#2906,#2907,#2908,#2909));
#751=EDGE_LOOP('',(#2910,#2911,#2912,#2913));
#752=EDGE_LOOP('',(#2914,#2915,#2916,#2917));
#753=EDGE_LOOP('',(#2918,#2919,#2920,#2921));
#754=EDGE_LOOP('',(#2922,#2923,#2924,#2925));
#755=EDGE_LOOP('',(#2926,#2927,#2928,#2929,#2930));
#756=EDGE_LOOP('',(#2931,#2932,#2933,#2934));
#757=EDGE_LOOP('',(#2935,#2936,#2937,#2938));
#758=EDGE_LOOP('',(#2939,#2940,#2941,#2942));
#759=EDGE_LOOP('',(#2943,#2944,#2945,#2946));
#760=EDGE_LOOP('',(#2947,#2948,#2949,#2950));
#761=EDGE_LOOP('',(#2951,#2952,#2953,#2954,#2955));
#762=EDGE_LOOP('',(#2956,#2957,#2958));
#763=EDGE_LOOP('',(#2959,#2960,#2961,#2962));
#764=EDGE_LOOP('',(#2963));
#765=EDGE_LOOP('',(#2964,#2965,#2966,#2967,#2968,#2969,#2970,#2971));
#766=EDGE_LOOP('',(#2972));
#767=EDGE_LOOP('',(#2973,#2974,#2975,#2976));
#768=EDGE_LOOP('',(#2977,#2978,#2979,#2980));
#769=EDGE_LOOP('',(#2981));
#770=EDGE_LOOP('',(#2982,#2983,#2984,#2985));
#771=EDGE_LOOP('',(#2986));
#772=EDGE_LOOP('',(#2987,#2988,#2989,#2990));
#773=EDGE_LOOP('',(#2991,#2992,#2993,#2994));
#774=EDGE_LOOP('',(#2995,#2996,#2997,#2998));
#775=EDGE_LOOP('',(#2999,#3000,#3001,#3002));
#776=EDGE_LOOP('',(#3003,#3004,#3005,#3006));
#777=EDGE_LOOP('',(#3007,#3008,#3009,#3010));
#778=EDGE_LOOP('',(#3011,#3012,#3013,#3014,#3015,#3016));
#779=EDGE_LOOP('',(#3017,#3018,#3019,#3020,#3021,#3022,#3023,#3024,#3025,
#3026,#3027,#3028,#3029,#3030,#3031,#3032,#3033,#3034));
#780=EDGE_LOOP('',(#3035,#3036,#3037,#3038,#3039));
#781=EDGE_LOOP('',(#3040,#3041,#3042,#3043));
#782=EDGE_LOOP('',(#3044,#3045,#3046,#3047,#3048));
#783=EDGE_LOOP('',(#3049,#3050,#3051,#3052,#3053,#3054));
#784=EDGE_LOOP('',(#3055,#3056,#3057,#3058,#3059,#3060,#3061,#3062));
#785=EDGE_LOOP('',(#3063,#3064,#3065,#3066,#3067,#3068,#3069,#3070,#3071,
#3072,#3073,#3074,#3075,#3076,#3077,#3078,#3079,#3080,#3081));
#786=EDGE_LOOP('',(#3082,#3083,#3084,#3085,#3086,#3087,#3088,#3089,#3090,
#3091,#3092,#3093,#3094,#3095,#3096,#3097,#3098,#3099,#3100));
#787=EDGE_LOOP('',(#3101,#3102,#3103,#3104));
#788=EDGE_LOOP('',(#3105));
#789=EDGE_LOOP('',(#3106,#3107,#3108,#3109,#3110));
#790=EDGE_LOOP('',(#3111,#3112,#3113,#3114,#3115));
#791=EDGE_LOOP('',(#3116,#3117,#3118,#3119,#3120));
#792=EDGE_LOOP('',(#3121));
#793=EDGE_LOOP('',(#3122));
#794=EDGE_LOOP('',(#3123,#3124,#3125,#3126));
#795=EDGE_LOOP('',(#3127));
#796=EDGE_LOOP('',(#3128));
#797=EDGE_LOOP('',(#3129,#3130,#3131,#3132));
#798=EDGE_LOOP('',(#3133,#3134,#3135,#3136,#3137,#3138));
#799=EDGE_LOOP('',(#3139,#3140,#3141,#3142));
#800=EDGE_LOOP('',(#3143));
#801=EDGE_LOOP('',(#3144));
#802=EDGE_LOOP('',(#3145,#3146,#3147,#3148));
#803=EDGE_LOOP('',(#3149,#3150,#3151,#3152));
#804=EDGE_LOOP('',(#3153,#3154));
#805=EDGE_LOOP('',(#3155,#3156,#3157,#3158));
#806=EDGE_LOOP('',(#3159,#3160,#3161,#3162));
#807=EDGE_LOOP('',(#3163,#3164,#3165,#3166));
#808=EDGE_LOOP('',(#3167,#3168,#3169,#3170));
#809=EDGE_LOOP('',(#3171,#3172,#3173,#3174));
#810=EDGE_LOOP('',(#3175));
#811=EDGE_LOOP('',(#3176));
#812=EDGE_LOOP('',(#3177,#3178,#3179,#3180));
#813=EDGE_LOOP('',(#3181));
#814=EDGE_LOOP('',(#3182));
#815=EDGE_LOOP('',(#3183,#3184,#3185,#3186));
#816=EDGE_LOOP('',(#3187,#3188,#3189,#3190));
#817=EDGE_LOOP('',(#3191,#3192,#3193,#3194));
#818=EDGE_LOOP('',(#3195,#3196,#3197,#3198));
#819=EDGE_LOOP('',(#3199,#3200,#3201,#3202));
#820=EDGE_LOOP('',(#3203));
#821=EDGE_LOOP('',(#3204));
#822=EDGE_LOOP('',(#3205,#3206,#3207,#3208));
#823=EDGE_LOOP('',(#3209));
#824=EDGE_LOOP('',(#3210));
#825=EDGE_LOOP('',(#3211,#3212,#3213,#3214));
#826=EDGE_LOOP('',(#3215,#3216));
#827=EDGE_LOOP('',(#3217));
#828=EDGE_LOOP('',(#3218));
#829=EDGE_LOOP('',(#3219,#3220,#3221,#3222));
#830=EDGE_LOOP('',(#3223,#3224,#3225,#3226));
#831=EDGE_LOOP('',(#3227));
#832=EDGE_LOOP('',(#3228,#3229,#3230,#3231));
#833=EDGE_LOOP('',(#3232));
#834=EDGE_LOOP('',(#3233,#3234,#3235,#3236,#3237,#3238,#3239,#3240,#3241,
#3242));
#835=EDGE_LOOP('',(#3243,#3244));
#836=EDGE_LOOP('',(#3245,#3246,#3247,#3248));
#837=EDGE_LOOP('',(#3249,#3250,#3251,#3252));
#838=EDGE_LOOP('',(#3253,#3254,#3255,#3256,#3257,#3258));
#839=EDGE_LOOP('',(#3259,#3260,#3261,#3262,#3263,#3264));
#840=EDGE_LOOP('',(#3265,#3266,#3267,#3268));
#841=EDGE_LOOP('',(#3269,#3270,#3271,#3272,#3273,#3274));
#842=EDGE_LOOP('',(#3275,#3276,#3277,#3278));
#843=EDGE_LOOP('',(#3279,#3280,#3281,#3282));
#844=EDGE_LOOP('',(#3283,#3284,#3285,#3286,#3287,#3288));
#845=EDGE_LOOP('',(#3289,#3290,#3291,#3292,#3293,#3294));
#846=EDGE_LOOP('',(#3295,#3296,#3297,#3298));
#847=EDGE_LOOP('',(#3299,#3300,#3301,#3302));
#848=EDGE_LOOP('',(#3303,#3304,#3305,#3306));
#849=EDGE_LOOP('',(#3307,#3308,#3309,#3310));
#850=EDGE_LOOP('',(#3311,#3312,#3313,#3314,#3315));
#851=EDGE_LOOP('',(#3316,#3317,#3318,#3319));
#852=EDGE_LOOP('',(#3320,#3321,#3322,#3323));
#853=EDGE_LOOP('',(#3324,#3325,#3326,#3327));
#854=EDGE_LOOP('',(#3328,#3329,#3330,#3331));
#855=EDGE_LOOP('',(#3332,#3333,#3334,#3335));
#856=EDGE_LOOP('',(#3336,#3337,#3338,#3339));
#857=EDGE_LOOP('',(#3340,#3341,#3342,#3343));
#858=EDGE_LOOP('',(#3344,#3345,#3346,#3347));
#859=EDGE_LOOP('',(#3348,#3349,#3350,#3351,#3352));
#860=EDGE_LOOP('',(#3353,#3354,#3355,#3356));
#861=EDGE_LOOP('',(#3357,#3358,#3359,#3360,#3361));
#862=EDGE_LOOP('',(#3362,#3363,#3364,#3365,#3366));
#863=EDGE_LOOP('',(#3367));
#864=EDGE_LOOP('',(#3368,#3369,#3370,#3371));
#865=EDGE_LOOP('',(#3372));
#866=EDGE_LOOP('',(#3373));
#867=EDGE_LOOP('',(#3374,#3375,#3376,#3377));
#868=EDGE_LOOP('',(#3378,#3379,#3380,#3381));
#869=EDGE_LOOP('',(#3382,#3383,#3384,#3385));
#870=EDGE_LOOP('',(#3386));
#871=EDGE_LOOP('',(#3387));
#872=EDGE_LOOP('',(#3388,#3389,#3390,#3391,#3392,#3393,#3394,#3395,#3396,
#3397,#3398,#3399,#3400,#3401,#3402,#3403,#3404,#3405,#3406,#3407,#3408,
#3409,#3410,#3411,#3412,#3413,#3414,#3415,#3416,#3417,#3418,#3419,#3420,
#3421,#3422,#3423,#3424,#3425));
#873=EDGE_LOOP('',(#3426,#3427,#3428,#3429,#3430,#3431));
#874=EDGE_LOOP('',(#3432,#3433,#3434,#3435,#3436,#3437,#3438,#3439,#3440,
#3441,#3442,#3443,#3444,#3445,#3446,#3447,#3448,#3449,#3450,#3451,#3452,
#3453,#3454,#3455,#3456,#3457,#3458,#3459,#3460,#3461,#3462,#3463,#3464,
#3465,#3466,#3467,#3468,#3469,#3470));
#875=EDGE_LOOP('',(#3471,#3472,#3473,#3474,#3475));
#876=EDGE_LOOP('',(#3476,#3477,#3478,#3479));
#877=EDGE_LOOP('',(#3480,#3481,#3482,#3483));
#878=EDGE_LOOP('',(#3484));
#879=EDGE_LOOP('',(#3485));
#880=EDGE_LOOP('',(#3486,#3487,#3488,#3489));
#881=EDGE_LOOP('',(#3490,#3491,#3492,#3493));
#882=EDGE_LOOP('',(#3494));
#883=EDGE_LOOP('',(#3495));
#884=EDGE_LOOP('',(#3496,#3497,#3498,#3499));
#885=EDGE_LOOP('',(#3500));
#886=EDGE_LOOP('',(#3501));
#887=EDGE_LOOP('',(#3502,#3503,#3504,#3505));
#888=EDGE_LOOP('',(#3506,#3507,#3508,#3509));
#889=EDGE_LOOP('',(#3510));
#890=EDGE_LOOP('',(#3511));
#891=EDGE_LOOP('',(#3512,#3513,#3514,#3515));
#892=EDGE_LOOP('',(#3516,#3517,#3518,#3519));
#893=EDGE_LOOP('',(#3520,#3521,#3522,#3523));
#894=EDGE_LOOP('',(#3524,#3525,#3526,#3527));
#895=EDGE_LOOP('',(#3528));
#896=EDGE_LOOP('',(#3529));
#897=EDGE_LOOP('',(#3530,#3531,#3532,#3533));
#898=EDGE_LOOP('',(#3534,#3535,#3536,#3537));
#899=EDGE_LOOP('',(#3538));
#900=EDGE_LOOP('',(#3539));
#901=EDGE_LOOP('',(#3540,#3541,#3542,#3543));
#902=EDGE_LOOP('',(#3544));
#903=EDGE_LOOP('',(#3545));
#904=EDGE_LOOP('',(#3546,#3547,#3548,#3549));
#905=EDGE_LOOP('',(#3550));
#906=EDGE_LOOP('',(#3551,#3552,#3553,#3554));
#907=EDGE_LOOP('',(#3555,#3556,#3557,#3558));
#908=EDGE_LOOP('',(#3559,#3560,#3561,#3562));
#909=EDGE_LOOP('',(#3563,#3564,#3565,#3566));
#910=EDGE_LOOP('',(#3567));
#911=EDGE_LOOP('',(#3568));
#912=EDGE_LOOP('',(#3569,#3570,#3571,#3572));
#913=EDGE_LOOP('',(#3573));
#914=EDGE_LOOP('',(#3574));
#915=LINE('',#5177,#1091);
#916=LINE('',#5193,#1092);
#917=LINE('',#5199,#1093);
#918=LINE('',#5258,#1094);
#919=LINE('',#5265,#1095);
#920=LINE('',#5267,#1096);
#921=LINE('',#5269,#1097);
#922=LINE('',#5270,#1098);
#923=LINE('',#5273,#1099);
#924=LINE('',#5275,#1100);
#925=LINE('',#5276,#1101);
#926=LINE('',#5279,#1102);
#927=LINE('',#5281,#1103);
#928=LINE('',#5282,#1104);
#929=LINE('',#5285,#1105);
#930=LINE('',#5287,#1106);
#931=LINE('',#5288,#1107);
#932=LINE('',#5291,#1108);
#933=LINE('',#5293,#1109);
#934=LINE('',#5294,#1110);
#935=LINE('',#5296,#1111);
#936=LINE('',#5297,#1112);
#937=LINE('',#5341,#1113);
#938=LINE('',#5383,#1114);
#939=LINE('',#5391,#1115);
#940=LINE('',#5395,#1116);
#941=LINE('',#5398,#1117);
#942=LINE('',#5406,#1118);
#943=LINE('',#5413,#1119);
#944=LINE('',#5461,#1120);
#945=LINE('',#5477,#1121);
#946=LINE('',#5483,#1122);
#947=LINE('',#5542,#1123);
#948=LINE('',#5549,#1124);
#949=LINE('',#5551,#1125);
#950=LINE('',#5553,#1126);
#951=LINE('',#5554,#1127);
#952=LINE('',#5557,#1128);
#953=LINE('',#5559,#1129);
#954=LINE('',#5560,#1130);
#955=LINE('',#5563,#1131);
#956=LINE('',#5565,#1132);
#957=LINE('',#5566,#1133);
#958=LINE('',#5569,#1134);
#959=LINE('',#5571,#1135);
#960=LINE('',#5572,#1136);
#961=LINE('',#5575,#1137);
#962=LINE('',#5577,#1138);
#963=LINE('',#5578,#1139);
#964=LINE('',#5580,#1140);
#965=LINE('',#5581,#1141);
#966=LINE('',#5597,#1142);
#967=LINE('',#5606,#1143);
#968=LINE('',#5617,#1144);
#969=LINE('',#5628,#1145);
#970=LINE('',#5639,#1146);
#971=LINE('',#5650,#1147);
#972=LINE('',#5661,#1148);
#973=LINE('',#5672,#1149);
#974=LINE('',#5683,#1150);
#975=LINE('',#5694,#1151);
#976=LINE('',#5705,#1152);
#977=LINE('',#5716,#1153);
#978=LINE('',#5727,#1154);
#979=LINE('',#5738,#1155);
#980=LINE('',#5740,#1156);
#981=LINE('',#5749,#1157);
#982=LINE('',#5760,#1158);
#983=LINE('',#5771,#1159);
#984=LINE('',#5782,#1160);
#985=LINE('',#5793,#1161);
#986=LINE('',#5804,#1162);
#987=LINE('',#5815,#1163);
#988=LINE('',#5826,#1164);
#989=LINE('',#5837,#1165);
#990=LINE('',#5848,#1166);
#991=LINE('',#5859,#1167);
#992=LINE('',#5870,#1168);
#993=LINE('',#5880,#1169);
#994=LINE('',#5891,#1170);
#995=LINE('',#5902,#1171);
#996=LINE('',#5913,#1172);
#997=LINE('',#5924,#1173);
#998=LINE('',#5935,#1174);
#999=LINE('',#5946,#1175);
#1000=LINE('',#5957,#1176);
#1001=LINE('',#5968,#1177);
#1002=LINE('',#5979,#1178);
#1003=LINE('',#5990,#1179);
#1004=LINE('',#6001,#1180);
#1005=LINE('',#6012,#1181);
#1006=LINE('',#6023,#1182);
#1007=LINE('',#6025,#1183);
#1008=LINE('',#6034,#1184);
#1009=LINE('',#6045,#1185);
#1010=LINE('',#6056,#1186);
#1011=LINE('',#6067,#1187);
#1012=LINE('',#6078,#1188);
#1013=LINE('',#6089,#1189);
#1014=LINE('',#6100,#1190);
#1015=LINE('',#6111,#1191);
#1016=LINE('',#6122,#1192);
#1017=LINE('',#6133,#1193);
#1018=LINE('',#6144,#1194);
#1019=LINE('',#6155,#1195);
#1020=LINE('',#6166,#1196);
#1021=LINE('',#6176,#1197);
#1022=LINE('',#7620,#1198);
#1023=LINE('',#7633,#1199);
#1024=LINE('',#7645,#1200);
#1025=LINE('',#7975,#1201);
#1026=LINE('',#8319,#1202);
#1027=LINE('',#8653,#1203);
#1028=LINE('',#8983,#1204);
#1029=LINE('',#9319,#1205);
#1030=LINE('',#14727,#1206);
#1031=LINE('',#15524,#1207);
#1032=LINE('',#15534,#1208);
#1033=LINE('',#15541,#1209);
#1034=LINE('',#15583,#1210);
#1035=LINE('',#15625,#1211);
#1036=LINE('',#15634,#1212);
#1037=LINE('',#15639,#1213);
#1038=LINE('',#15642,#1214);
#1039=LINE('',#15645,#1215);
#1040=LINE('',#15649,#1216);
#1041=LINE('',#15653,#1217);
#1042=LINE('',#15657,#1218);
#1043=LINE('',#15664,#1219);
#1044=LINE('',#15671,#1220);
#1045=LINE('',#15675,#1221);
#1046=LINE('',#15679,#1222);
#1047=LINE('',#15683,#1223);
#1048=LINE('',#15687,#1224);
#1049=LINE('',#15694,#1225);
#1050=LINE('',#15699,#1226);
#1051=LINE('',#15710,#1227);
#1052=LINE('',#15722,#1228);
#1053=LINE('',#15863,#1229);
#1054=LINE('',#15978,#1230);
#1055=LINE('',#16402,#1231);
#1056=LINE('',#16802,#1232);
#1057=LINE('',#17236,#1233);
#1058=LINE('',#17648,#1234);
#1059=LINE('',#18052,#1235);
#1060=LINE('',#18470,#1236);
#1061=LINE('',#18872,#1237);
#1062=LINE('',#19296,#1238);
#1063=LINE('',#19720,#1239);
#1064=LINE('',#20146,#1240);
#1065=LINE('',#20554,#1241);
#1066=LINE('',#20960,#1242);
#1067=LINE('',#21259,#1243);
#1068=LINE('',#21635,#1244);
#1069=LINE('',#22036,#1245);
#1070=LINE('',#22418,#1246);
#1071=LINE('',#22804,#1247);
#1072=LINE('',#23196,#1248);
#1073=LINE('',#23578,#1249);
#1074=LINE('',#23968,#1250);
#1075=LINE('',#24346,#1251);
#1076=LINE('',#24732,#1252);
#1077=LINE('',#25116,#1253);
#1078=LINE('',#25507,#1254);
#1079=LINE('',#26142,#1255);
#1080=LINE('',#26496,#1256);
#1081=LINE('',#27575,#1257);
#1082=LINE('',#27586,#1258);
#1083=LINE('',#27604,#1259);
#1084=LINE('',#27617,#1260);
#1085=LINE('',#27634,#1261);
#1086=LINE('',#27654,#1262);
#1087=LINE('',#27656,#1263);
#1088=LINE('',#27658,#1264);
#1089=LINE('',#27664,#1265);
#1090=LINE('',#27672,#1266);
#1091=VECTOR('',#4292,10.);
#1092=VECTOR('',#4293,10.);
#1093=VECTOR('',#4300,10.);
#1094=VECTOR('',#4301,10.);
#1095=VECTOR('',#4310,10.);
#1096=VECTOR('',#4311,10.);
#1097=VECTOR('',#4312,10.);
#1098=VECTOR('',#4313,10.);
#1099=VECTOR('',#4316,9.99999999999998);
#1100=VECTOR('',#4317,9.99999999999998);
#1101=VECTOR('',#4318,10.);
#1102=VECTOR('',#4321,10.);
#1103=VECTOR('',#4322,10.);
#1104=VECTOR('',#4323,10.);
#1105=VECTOR('',#4326,10.);
#1106=VECTOR('',#4327,10.);
#1107=VECTOR('',#4328,10.);
#1108=VECTOR('',#4331,10.);
#1109=VECTOR('',#4332,10.);
#1110=VECTOR('',#4333,10.);
#1111=VECTOR('',#4336,10.);
#1112=VECTOR('',#4337,10.);
#1113=VECTOR('',#4346,0.999999999999996);
#1114=VECTOR('',#4351,4.75);
#1115=VECTOR('',#4362,7.269);
#1116=VECTOR('',#4367,7.528);
#1117=VECTOR('',#4370,6.974);
#1118=VECTOR('',#4381,3.7);
#1119=VECTOR('',#4390,2.204);
#1120=VECTOR('',#4395,10.);
#1121=VECTOR('',#4396,10.);
#1122=VECTOR('',#4403,10.);
#1123=VECTOR('',#4404,10.);
#1124=VECTOR('',#4413,10.);
#1125=VECTOR('',#4414,10.);
#1126=VECTOR('',#4415,10.);
#1127=VECTOR('',#4416,10.);
#1128=VECTOR('',#4419,9.99999999999998);
#1129=VECTOR('',#4420,9.99999999999998);
#1130=VECTOR('',#4421,10.);
#1131=VECTOR('',#4424,10.);
#1132=VECTOR('',#4425,10.);
#1133=VECTOR('',#4426,10.);
#1134=VECTOR('',#4429,10.);
#1135=VECTOR('',#4430,10.);
#1136=VECTOR('',#4431,10.);
#1137=VECTOR('',#4434,10.);
#1138=VECTOR('',#4435,10.);
#1139=VECTOR('',#4436,10.);
#1140=VECTOR('',#4439,10.);
#1141=VECTOR('',#4440,10.);
#1142=VECTOR('',#4449,10.);
#1143=VECTOR('',#4450,10.);
#1144=VECTOR('',#4451,10.);
#1145=VECTOR('',#4452,10.);
#1146=VECTOR('',#4453,10.);
#1147=VECTOR('',#4454,10.);
#1148=VECTOR('',#4455,10.);
#1149=VECTOR('',#4456,10.);
#1150=VECTOR('',#4457,10.);
#1151=VECTOR('',#4458,10.);
#1152=VECTOR('',#4459,10.);
#1153=VECTOR('',#4460,10.);
#1154=VECTOR('',#4461,10.);
#1155=VECTOR('',#4462,10.);
#1156=VECTOR('',#4463,10.);
#1157=VECTOR('',#4464,10.);
#1158=VECTOR('',#4465,10.);
#1159=VECTOR('',#4466,10.);
#1160=VECTOR('',#4467,10.);
#1161=VECTOR('',#4468,10.);
#1162=VECTOR('',#4469,10.);
#1163=VECTOR('',#4470,10.);
#1164=VECTOR('',#4471,10.);
#1165=VECTOR('',#4472,10.);
#1166=VECTOR('',#4473,10.);
#1167=VECTOR('',#4474,10.);
#1168=VECTOR('',#4475,10.);
#1169=VECTOR('',#4476,10.);
#1170=VECTOR('',#4479,10.);
#1171=VECTOR('',#4480,10.);
#1172=VECTOR('',#4481,10.);
#1173=VECTOR('',#4482,10.);
#1174=VECTOR('',#4483,10.);
#1175=VECTOR('',#4484,10.);
#1176=VECTOR('',#4485,10.);
#1177=VECTOR('',#4486,10.);
#1178=VECTOR('',#4487,10.);
#1179=VECTOR('',#4488,10.);
#1180=VECTOR('',#4489,10.);
#1181=VECTOR('',#4490,10.);
#1182=VECTOR('',#4491,10.);
#1183=VECTOR('',#4492,10.);
#1184=VECTOR('',#4493,10.);
#1185=VECTOR('',#4494,10.);
#1186=VECTOR('',#4495,10.);
#1187=VECTOR('',#4496,10.);
#1188=VECTOR('',#4497,10.);
#1189=VECTOR('',#4498,10.);
#1190=VECTOR('',#4499,10.);
#1191=VECTOR('',#4500,10.);
#1192=VECTOR('',#4501,10.);
#1193=VECTOR('',#4502,10.);
#1194=VECTOR('',#4503,10.);
#1195=VECTOR('',#4504,10.);
#1196=VECTOR('',#4505,10.);
#1197=VECTOR('',#4506,10.);
#1198=VECTOR('',#4583,5.);
#1199=VECTOR('',#4602,6.40732538114918);
#1200=VECTOR('',#4619,3.72275);
#1201=VECTOR('',#4624,3.72275);
#1202=VECTOR('',#4627,3.72275);
#1203=VECTOR('',#4630,3.72275);
#1204=VECTOR('',#4633,3.72275);
#1205=VECTOR('',#4636,3.72275);
#1206=VECTOR('',#4663,2.204);
#1207=VECTOR('',#4670,5.42440960677665);
#1208=VECTOR('',#4685,7.27835105742136);
#1209=VECTOR('',#4694,7.52835105742136);
#1210=VECTOR('',#4699,0.999999999999999);
#1211=VECTOR('',#4704,5.);
#1212=VECTOR('',#4715,7.20746054905241);
#1213=VECTOR('',#4722,7.52312685038423);
#1214=VECTOR('',#4725,7.36529369971832);
#1215=VECTOR('',#4730,7.36790580323689);
#1216=VECTOR('',#4735,6.41628586403442);
#1217=VECTOR('',#4740,6.40969108660508);
#1218=VECTOR('',#4745,6.40906719549494);
#1219=VECTOR('',#4754,6.41550316824698);
#1220=VECTOR('',#4763,6.40820475053297);
#1221=VECTOR('',#4768,6.40787078036307);
#1222=VECTOR('',#4773,6.40732538114918);
#1223=VECTOR('',#4778,6.40706623219228);
#1224=VECTOR('',#4783,6.40667124022599);
#1225=VECTOR('',#4792,4.66385643997278);
#1226=VECTOR('',#4799,3.44589712386029);
#1227=VECTOR('',#4814,6.40906719549494);
#1228=VECTOR('',#4831,2.204);
#1229=VECTOR('',#4834,2.204);
#1230=VECTOR('',#4841,2.204);
#1231=VECTOR('',#4844,2.204);
#1232=VECTOR('',#4847,2.204);
#1233=VECTOR('',#4850,2.204);
#1234=VECTOR('',#4853,2.204);
#1235=VECTOR('',#4856,2.204);
#1236=VECTOR('',#4859,2.204);
#1237=VECTOR('',#4862,2.204);
#1238=VECTOR('',#4865,2.204);
#1239=VECTOR('',#4868,2.204);
#1240=VECTOR('',#4871,2.204);
#1241=VECTOR('',#4874,2.204);
#1242=VECTOR('',#4877,1.77625);
#1243=VECTOR('',#4882,1.77625);
#1244=VECTOR('',#4885,1.77625);
#1245=VECTOR('',#4888,1.77625);
#1246=VECTOR('',#4891,1.77625);
#1247=VECTOR('',#4894,1.77625);
#1248=VECTOR('',#4897,1.77625);
#1249=VECTOR('',#4900,1.77625);
#1250=VECTOR('',#4903,1.77625);
#1251=VECTOR('',#4906,1.77625);
#1252=VECTOR('',#4909,1.77625);
#1253=VECTOR('',#4912,1.77625);
#1254=VECTOR('',#4915,1.77625);
#1255=VECTOR('',#4924,0.999999999999996);
#1256=VECTOR('',#4947,6.40820475053297);
#1257=VECTOR('',#4972,4.48902817623056);
#1258=VECTOR('',#4987,6.40950758978419);
#1259=VECTOR('',#5012,6.40867450936473);
#1260=VECTOR('',#5031,6.40772765523458);
#1261=VECTOR('',#5054,6.40690599146347);
#1262=VECTOR('',#5083,4.42329516333974);
#1263=VECTOR('',#5086,2.21164758166987);
#1264=VECTOR('',#5089,2.21164758166987);
#1265=VECTOR('',#5096,3.7);
#1266=VECTOR('',#5107,2.204);
#1267=B_SPLINE_CURVE_WITH_KNOTS('',3,(#5162,#5163,#5164,#5165,#5166,#5167,
#5168,#5169,#5170,#5171,#5172,#5173,#5174,#5175),.UNSPECIFIED.,.F.,.F.,
(4,2,2,2,2,2,4),(-0.844212290556731,-0.730966332817565,-0.619975754240938,
-0.457326579004558,-0.29977928179387,-0.147336283383114,0.),
 .UNSPECIFIED.);
#1268=B_SPLINE_CURVE_WITH_KNOTS('',3,(#5179,#5180,#5181,#5182,#5183,#5184,
#5185,#5186,#5187,#5188,#5189,#5190,#5191,#5192),.UNSPECIFIED.,.F.,.F.,
(4,2,2,2,2,2,4),(-0.844212290556731,-0.730966332817565,-0.619975754240938,
-0.457326579004558,-0.29977928179387,-0.147336283383114,0.),
 .UNSPECIFIED.);
#1269=B_SPLINE_CURVE_WITH_KNOTS('',3,(#5229,#5230,#5231,#5232,#5233,#5234,
#5235,#5236,#5237,#5238,#5239,#5240,#5241,#5242),.UNSPECIFIED.,.F.,.F.,
(4,2,2,2,2,2,4),(-0.847325527525843,-0.749719327139836,-0.649860858750851,
-0.495073659399383,-0.335166304629316,-0.170141007879843,0.),
 .UNSPECIFIED.);
#1270=B_SPLINE_CURVE_WITH_KNOTS('',3,(#5244,#5245,#5246,#5247,#5248,#5249,
#5250,#5251,#5252,#5253,#5254,#5255,#5256,#5257),.UNSPECIFIED.,.F.,.F.,
(4,2,2,2,2,2,4),(-0.847325527525843,-0.749719327139836,-0.649860858750851,
-0.495073659399383,-0.335166304629316,-0.170141007879843,0.),
 .UNSPECIFIED.);
#1271=B_SPLINE_CURVE_WITH_KNOTS('',3,(#5304,#5305,#5306,#5307,#5308,#5309,
#5310,#5311,#5312,#5313,#5314,#5315,#5316,#5317,#5318,#5319,#5320,#5321,
#5322,#5323,#5324,#5325,#5326,#5327,#5328,#5329),.UNSPECIFIED.,.F.,.F.,
(4,2,2,2,2,2,2,2,2,2,2,2,4),(-0.604649456116834,-0.566857559730589,-0.529065663344343,
-0.491276377715985,-0.453487092087626,-0.415697806459267,-0.377908520830908,
-0.340116624444663,-0.302324728058417,-0.264532831672172,-0.226740935285926,
-0.188951649657567,-0.151162364029209),.UNSPECIFIED.);
#1272=B_SPLINE_CURVE_WITH_KNOTS('',3,(#5330,#5331,#5332,#5333,#5334,#5335,
#5336,#5337,#5338,#5339),.UNSPECIFIED.,.F.,.F.,(4,2,2,2,4),(-0.151162364029209,
-0.11337307840085,-0.0755837927724912,-0.0377918963862456,0.),
 .UNSPECIFIED.);
#1273=B_SPLINE_CURVE_WITH_KNOTS('',3,(#5343,#5344,#5345,#5346,#5347,#5348,
#5349,#5350,#5351,#5352),.UNSPECIFIED.,.F.,.F.,(4,2,2,2,4),(0.,0.037716777501004,
0.075433555002008,0.113149929875281,0.150866304748554),.UNSPECIFIED.);
#1274=B_SPLINE_CURVE_WITH_KNOTS('',3,(#5353,#5354,#5355,#5356,#5357,#5358,
#5359,#5360,#5361,#5362,#5363,#5364,#5365,#5366,#5367,#5368,#5369,#5370,
#5371,#5372,#5373,#5374,#5375,#5376,#5377,#5378),.UNSPECIFIED.,.F.,.F.,
(4,2,2,2,2,2,2,2,2,2,2,2,4),(0.150866304748554,0.188582679621827,0.2262990544951,
0.264015831996104,0.301732609497108,0.339449386998112,0.377166164499116,
0.414882539372389,0.452598914245662,0.490315289118935,0.528031663992208,
0.565748441493212,0.603465218994216),.UNSPECIFIED.);
#1275=B_SPLINE_CURVE_WITH_KNOTS('',3,(#5446,#5447,#5448,#5449,#5450,#5451,
#5452,#5453,#5454,#5455,#5456,#5457,#5458,#5459),.UNSPECIFIED.,.F.,.F.,
(4,2,2,2,2,2,4),(-0.844212290556731,-0.730966332817565,-0.619975754240938,
-0.457326579004558,-0.29977928179387,-0.147336283383114,0.),
 .UNSPECIFIED.);
#1276=B_SPLINE_CURVE_WITH_KNOTS('',3,(#5463,#5464,#5465,#5466,#5467,#5468,
#5469,#5470,#5471,#5472,#5473,#5474,#5475,#5476),.UNSPECIFIED.,.F.,.F.,
(4,2,2,2,2,2,4),(-0.844212290556731,-0.730966332817565,-0.619975754240938,
-0.457326579004558,-0.29977928179387,-0.147336283383114,0.),
 .UNSPECIFIED.);
#1277=B_SPLINE_CURVE_WITH_KNOTS('',3,(#5513,#5514,#5515,#5516,#5517,#5518,
#5519,#5520,#5521,#5522,#5523,#5524,#5525,#5526),.UNSPECIFIED.,.F.,.F.,
(4,2,2,2,2,2,4),(-0.847325527525843,-0.749719327139836,-0.649860858750851,
-0.495073659399383,-0.335166304629316,-0.170141007879843,0.),
 .UNSPECIFIED.);
#1278=B_SPLINE_CURVE_WITH_KNOTS('',3,(#5528,#5529,#5530,#5531,#5532,#5533,
#5534,#5535,#5536,#5537,#5538,#5539,#5540,#5541),.UNSPECIFIED.,.F.,.F.,
(4,2,2,2,2,2,4),(-0.847325527525843,-0.749719327139836,-0.649860858750851,
-0.495073659399383,-0.335166304629316,-0.170141007879843,0.),
 .UNSPECIFIED.);
#1279=B_SPLINE_CURVE_WITH_KNOTS('',3,(#5588,#5589,#5590,#5591,#5592,#5593,
#5594,#5595),.UNSPECIFIED.,.F.,.F.,(4,2,2,4),(0.,0.000697892015497008,0.0143255677369775,
0.0286350340362092),.UNSPECIFIED.);
#1280=B_SPLINE_CURVE_WITH_KNOTS('',3,(#5599,#5600,#5601,#5602,#5603,#5604),
 .UNSPECIFIED.,.F.,.F.,(4,2,4),(0.,0.0523373446002982,0.104355593610831),
 .UNSPECIFIED.);
#1281=B_SPLINE_CURVE_WITH_KNOTS('',3,(#5608,#5609,#5610,#5611,#5612,#5613,
#5614,#5615),.UNSPECIFIED.,.F.,.F.,(4,2,2,4),(0.,0.00526521584710592,0.0639602373511304,
0.128212067318051),.UNSPECIFIED.);
#1282=B_SPLINE_CURVE_WITH_KNOTS('',3,(#5619,#5620,#5621,#5622,#5623,#5624,
#5625,#5626),.UNSPECIFIED.,.F.,.F.,(4,2,2,4),(0.,0.0627475271162915,0.120075061733582,
0.125236068694296),.UNSPECIFIED.);
#1283=B_SPLINE_CURVE_WITH_KNOTS('',3,(#5630,#5631,#5632,#5633,#5634,#5635,
#5636,#5637),.UNSPECIFIED.,.F.,.F.,(4,2,2,4),(0.,0.00526560282662867,0.0639612078258487,
0.128213120660444),.UNSPECIFIED.);
#1284=B_SPLINE_CURVE_WITH_KNOTS('',3,(#5641,#5642,#5643,#5644,#5645,#5646,
#5647,#5648),.UNSPECIFIED.,.F.,.F.,(4,2,2,4),(0.,0.0627475590562519,0.120075649624267,
0.125237044527633),.UNSPECIFIED.);
#1285=B_SPLINE_CURVE_WITH_KNOTS('',3,(#5652,#5653,#5654,#5655,#5656,#5657,
#5658,#5659),.UNSPECIFIED.,.F.,.F.,(4,2,2,4),(0.,0.00526602648868038,0.0639622680416072,
0.128214273235454),.UNSPECIFIED.);
#1286=B_SPLINE_CURVE_WITH_KNOTS('',3,(#5663,#5664,#5665,#5666,#5667,#5668,
#5669,#5670),.UNSPECIFIED.,.F.,.F.,(4,2,2,4),(0.,0.0627475953399776,0.120076292215752,
0.125238111923284),.UNSPECIFIED.);
#1287=B_SPLINE_CURVE_WITH_KNOTS('',3,(#5674,#5675,#5676,#5677,#5678,#5679,
#5680,#5681),.UNSPECIFIED.,.F.,.F.,(4,2,2,4),(0.,0.00526649276184272,0.0639634322919596,
0.128215541011568),.UNSPECIFIED.);
#1288=B_SPLINE_CURVE_WITH_KNOTS('',3,(#5685,#5686,#5687,#5688,#5689,#5690,
#5691,#5692),.UNSPECIFIED.,.F.,.F.,(4,2,2,4),(0.,0.0627476367935851,0.120076998293466,
0.125239285656593),.UNSPECIFIED.);
#1289=B_SPLINE_CURVE_WITH_KNOTS('',3,(#5696,#5697,#5698,#5699,#5700,#5701,
#5702,#5703),.UNSPECIFIED.,.F.,.F.,(4,2,2,4),(0.,0.00526700898296905,0.0639647182192301,
0.128216943693669),.UNSPECIFIED.);
#1290=B_SPLINE_CURVE_WITH_KNOTS('',3,(#5707,#5708,#5709,#5710,#5711,#5712,
#5713,#5714),.UNSPECIFIED.,.F.,.F.,(4,2,2,4),(0.,0.0627476844547414,0.120077778736361,
0.125240584036134),.UNSPECIFIED.);
#1291=B_SPLINE_CURVE_WITH_KNOTS('',3,(#5718,#5719,#5720,#5721,#5722,#5723,
#5724,#5725),.UNSPECIFIED.,.F.,.F.,(4,2,2,4),(0.,0.0052675843601308,0.0639661480124282,
0.12821850616927),.UNSPECIFIED.);
#1292=B_SPLINE_CURVE_WITH_KNOTS('',3,(#5729,#5730,#5731,#5732,#5733,#5734,
#5735,#5736),.UNSPECIFIED.,.F.,.F.,(4,2,2,4),(0.,0.0627497316200279,0.120007641766305,
0.125309768916132),.UNSPECIFIED.);
#1293=B_SPLINE_CURVE_WITH_KNOTS('',3,(#5742,#5743,#5744,#5745,#5746,#5747),
 .UNSPECIFIED.,.F.,.F.,(4,2,4),(1.75570920373614E-15,0.0320055376006011,
0.0638199285984987),.UNSPECIFIED.);
#1294=B_SPLINE_CURVE_WITH_KNOTS('',3,(#5751,#5752,#5753,#5754,#5755,#5756,
#5757,#5758),.UNSPECIFIED.,.F.,.F.,(4,2,2,4),(0.,0.00526977567755582,0.0639683005470083,
0.128217977351555),.UNSPECIFIED.);
#1295=B_SPLINE_CURVE_WITH_KNOTS('',3,(#5762,#5763,#5764,#5765,#5766,#5767,
#5768,#5769),.UNSPECIFIED.,.F.,.F.,(4,2,2,4),(0.,0.062761494454614,0.120090502459536,
0.125241025317951),.UNSPECIFIED.);
#1296=B_SPLINE_CURVE_WITH_KNOTS('',3,(#5773,#5774,#5775,#5776,#5777,#5778,
#5779,#5780),.UNSPECIFIED.,.F.,.F.,(4,2,2,4),(0.,0.00526922229267531,0.0639669243235216,
0.128216474527037),.UNSPECIFIED.);
#1297=B_SPLINE_CURVE_WITH_KNOTS('',3,(#5784,#5785,#5786,#5787,#5788,#5789,
#5790,#5791),.UNSPECIFIED.,.F.,.F.,(4,2,2,4),(0.,0.0627614441556716,0.120089692527127,
0.125239677665907),.UNSPECIFIED.);
#1298=B_SPLINE_CURVE_WITH_KNOTS('',3,(#5795,#5796,#5797,#5798,#5799,#5800,
#5801,#5802),.UNSPECIFIED.,.F.,.F.,(4,2,2,4),(0.,0.0052687245725873,0.0639656835644766,
0.128215122077758),.UNSPECIFIED.);
#1299=B_SPLINE_CURVE_WITH_KNOTS('',3,(#5806,#5807,#5808,#5809,#5810,#5811,
#5812,#5813),.UNSPECIFIED.,.F.,.F.,(4,2,2,4),(0.,0.0627614005096921,0.120088961436388,
0.125238462177896),.UNSPECIFIED.);
#1300=B_SPLINE_CURVE_WITH_KNOTS('',3,(#5817,#5818,#5819,#5820,#5821,#5822,
#5823,#5824),.UNSPECIFIED.,.F.,.F.,(4,2,2,4),(0.,0.00526827403022492,0.0639645578123657,
0.128213897069805),.UNSPECIFIED.);
#1301=B_SPLINE_CURVE_WITH_KNOTS('',3,(#5828,#5829,#5830,#5831,#5832,#5833,
#5834,#5835),.UNSPECIFIED.,.F.,.F.,(4,2,2,4),(0.,0.0627613623859368,0.12008829741618,
0.125237359044329),.UNSPECIFIED.);
#1302=B_SPLINE_CURVE_WITH_KNOTS('',3,(#5839,#5840,#5841,#5842,#5843,#5844,
#5845,#5846),.UNSPECIFIED.,.F.,.F.,(4,2,2,4),(0.,0.0052678638691292,0.0639635307055346,
0.128212781223319),.UNSPECIFIED.);
#1303=B_SPLINE_CURVE_WITH_KNOTS('',3,(#5850,#5851,#5852,#5853,#5854,#5855,
#5856,#5857),.UNSPECIFIED.,.F.,.F.,(4,2,2,4),(0.,0.0627613288883452,0.120087691004123,
0.125236352349363),.UNSPECIFIED.);
#1304=B_SPLINE_CURVE_WITH_KNOTS('',3,(#5861,#5862,#5863,#5864,#5865,#5866,
#5867,#5868),.UNSPECIFIED.,.F.,.F.,(4,2,2,4),(0.,0.00526748857527077,0.0639625889506368,
0.128211759700356),.UNSPECIFIED.);
#1305=B_SPLINE_CURVE_WITH_KNOTS('',3,(#5872,#5873,#5874,#5875,#5876,#5877,
#5878,#5879),.UNSPECIFIED.,.F.,.F.,(4,2,2,4),(0.,0.0627622351934734,0.120057633553872,
0.125268887079596),.UNSPECIFIED.);
#1306=B_SPLINE_CURVE_WITH_KNOTS('',3,(#5884,#5885,#5886,#5887,#5888,#5889),
 .UNSPECIFIED.,.F.,.F.,(4,2,4),(0.,0.0498589762945784,0.0999595266847454),
 .UNSPECIFIED.);
#1307=B_SPLINE_CURVE_WITH_KNOTS('',3,(#5893,#5894,#5895,#5896,#5897,#5898,
#5899,#5900),.UNSPECIFIED.,.F.,.F.,(4,2,2,4),(0.,0.0627475125621108,0.120074786005034,
0.125235611253279),.UNSPECIFIED.);
#1308=B_SPLINE_CURVE_WITH_KNOTS('',3,(#5904,#5905,#5906,#5907,#5908,#5909,
#5910,#5911),.UNSPECIFIED.,.F.,.F.,(4,2,2,4),(0.,0.00526540507665305,0.0639607121557458,
0.128212582461846),.UNSPECIFIED.);
#1309=B_SPLINE_CURVE_WITH_KNOTS('',3,(#5915,#5916,#5917,#5918,#5919,#5920,
#5921,#5922),.UNSPECIFIED.,.F.,.F.,(4,2,2,4),(0.,0.0627475425879394,0.120075349322764,
0.125236545975591),.UNSPECIFIED.);
#1310=B_SPLINE_CURVE_WITH_KNOTS('',3,(#5926,#5927,#5928,#5929,#5930,#5931,
#5932,#5933),.UNSPECIFIED.,.F.,.F.,(4,2,2,4),(0.,0.00526580973145337,0.0639617259034633,
0.128213683646694),.UNSPECIFIED.);
#1311=B_SPLINE_CURVE_WITH_KNOTS('',3,(#5937,#5938,#5939,#5940,#5941,#5942,
#5943,#5944),.UNSPECIFIED.,.F.,.F.,(4,2,2,4),(0.,0.0627475766076911,0.120075963575788,
0.12523756592846),.UNSPECIFIED.);
#1312=B_SPLINE_CURVE_WITH_KNOTS('',3,(#5948,#5949,#5950,#5951,#5952,#5953,
#5954,#5955),.UNSPECIFIED.,.F.,.F.,(4,2,2,4),(0.,0.00526625387771515,0.063962836142632,
0.128214891577853),.UNSPECIFIED.);
#1313=B_SPLINE_CURVE_WITH_KNOTS('',3,(#5959,#5960,#5961,#5962,#5963,#5964,
#5965,#5966),.UNSPECIFIED.,.F.,.F.,(4,2,2,4),(0.,0.0627476153613634,0.120076636694826,
0.12523868444785),.UNSPECIFIED.);
#1314=B_SPLINE_CURVE_WITH_KNOTS('',3,(#5970,#5971,#5972,#5973,#5974,#5975,
#5976,#5977),.UNSPECIFIED.,.F.,.F.,(4,2,2,4),(0.,0.00526674410433897,0.063964058787172,
0.128216224084347),.UNSPECIFIED.);
#1315=B_SPLINE_CURVE_WITH_KNOTS('',3,(#5981,#5982,#5983,#5984,#5985,#5986,
#5987,#5988),.UNSPECIFIED.,.F.,.F.,(4,2,2,4),(0.,0.0627476597736949,0.120077378440881,
0.125239917954739),.UNSPECIFIED.);
#1316=B_SPLINE_CURVE_WITH_KNOTS('',3,(#5992,#5993,#5994,#5995,#5996,#5997,
#5998,#5999),.UNSPECIFIED.,.F.,.F.,(4,2,2,4),(0.,0.00526728861301724,0.0639654135345664,
0.128217703164965),.UNSPECIFIED.);
#1317=B_SPLINE_CURVE_WITH_KNOTS('',3,(#6003,#6004,#6005,#6006,#6007,#6008,
#6009,#6010),.UNSPECIFIED.,.F.,.F.,(4,2,2,4),(0.,0.0627477110123208,0.120078200979348,
0.125241286926992),.UNSPECIFIED.);
#1318=B_SPLINE_CURVE_WITH_KNOTS('',3,(#6014,#6015,#6016,#6017,#6018,#6019,
#6020,#6021),.UNSPECIFIED.,.F.,.F.,(4,2,2,4),(0.,0.00526789777186566,0.0639669253649914,
0.128219356862823),.UNSPECIFIED.);
#1319=B_SPLINE_CURVE_WITH_KNOTS('',3,(#6027,#6028,#6029,#6030,#6031,#6032),
 .UNSPECIFIED.,.F.,.F.,(4,2,4),(0.,0.0322464693148723,0.0645605482559509),
 .UNSPECIFIED.);
#1320=B_SPLINE_CURVE_WITH_KNOTS('',3,(#6036,#6037,#6038,#6039,#6040,#6041,
#6042,#6043),.UNSPECIFIED.,.F.,.F.,(4,2,2,4),(0.,0.0627615225357567,0.12009094148456,
0.125241756269418),.UNSPECIFIED.);
#1321=B_SPLINE_CURVE_WITH_KNOTS('',3,(#6047,#6048,#6049,#6050,#6051,#6052,
#6053,#6054),.UNSPECIFIED.,.F.,.F.,(4,2,2,4),(0.,0.00526949141755586,0.0639675940491126,
0.128217205528332),.UNSPECIFIED.);
#1322=B_SPLINE_CURVE_WITH_KNOTS('',3,(#6058,#6059,#6060,#6061,#6062,#6063,
#6064,#6065),.UNSPECIFIED.,.F.,.F.,(4,2,2,4),(0.,0.0627614683917021,0.120090086793172,
0.125240333549308),.UNSPECIFIED.);
#1323=B_SPLINE_CURVE_WITH_KNOTS('',3,(#6069,#6070,#6071,#6072,#6073,#6074,
#6075,#6076),.UNSPECIFIED.,.F.,.F.,(4,2,2,4),(0.,0.00526896705103507,0.0639662884118339,
0.128215781088997),.UNSPECIFIED.);
#1324=B_SPLINE_CURVE_WITH_KNOTS('',3,(#6080,#6081,#6082,#6083,#6084,#6085,
#6086,#6087),.UNSPECIFIED.,.F.,.F.,(4,2,2,4),(0.,0.0627614215780341,0.120089317924044,
0.125239054744074),.UNSPECIFIED.);
#1325=B_SPLINE_CURVE_WITH_KNOTS('',3,(#6091,#6092,#6093,#6094,#6095,#6096,
#6097,#6098),.UNSPECIFIED.,.F.,.F.,(4,2,2,4),(0.,0.00526849386310405,0.0639651074163281,
0.128214494876759),.UNSPECIFIED.);
#1326=B_SPLINE_CURVE_WITH_KNOTS('',3,(#6102,#6103,#6104,#6105,#6106,#6107,
#6108,#6109),.UNSPECIFIED.,.F.,.F.,(4,2,2,4),(0.,0.0627613808182858,0.120088621680663,
0.125237897640557),.UNSPECIFIED.);
#1327=B_SPLINE_CURVE_WITH_KNOTS('',3,(#6113,#6114,#6115,#6116,#6117,#6118,
#6119,#6120),.UNSPECIFIED.,.F.,.F.,(4,2,2,4),(0.,0.00526806427303071,0.0639640328250225,
0.128213326505552),.UNSPECIFIED.);
#1328=B_SPLINE_CURVE_WITH_KNOTS('',3,(#6124,#6125,#6126,#6127,#6128,#6129,
#6130,#6131),.UNSPECIFIED.,.F.,.F.,(4,2,2,4),(0.,0.0627613451073725,0.120087987526447,
0.125236844511966),.UNSPECIFIED.);
#1329=B_SPLINE_CURVE_WITH_KNOTS('',3,(#6135,#6136,#6137,#6138,#6139,#6140,
#6141,#6142),.UNSPECIFIED.,.F.,.F.,(4,2,2,4),(0.,0.00526767216729547,0.0639630498969236,
0.128212259500237),.UNSPECIFIED.);
#1330=B_SPLINE_CURVE_WITH_KNOTS('',3,(#6146,#6147,#6148,#6149,#6150,#6151,
#6152,#6153),.UNSPECIFIED.,.F.,.F.,(4,2,2,4),(0.,0.0627613136441549,0.120087406937392,
0.125235881024186),.UNSPECIFIED.);
#1331=B_SPLINE_CURVE_WITH_KNOTS('',3,(#6157,#6158,#6159,#6160,#6161,#6162,
#6163,#6164),.UNSPECIFIED.,.F.,.F.,(4,2,2,4),(0.,0.00526731255574918,0.0639621465613893,
0.128211280360621),.UNSPECIFIED.);
#1332=B_SPLINE_CURVE_WITH_KNOTS('',3,(#6168,#6169,#6170,#6171,#6172,#6173,
#6174,#6175),.UNSPECIFIED.,.F.,.F.,(4,2,2,4),(0.,0.0104628362527636,0.0207308659069718,
0.0209057471409188),.UNSPECIFIED.);
#1333=B_SPLINE_CURVE_WITH_KNOTS('',3,(#6179,#6180,#6181,#6182,#6183,#6184,
#6185,#6186,#6187,#6188,#6189,#6190),.UNSPECIFIED.,.F.,.F.,(4,2,2,2,2,4),
(-0.347751064939877,-0.282575309839093,-0.217361093090031,-0.173962239844469,
-0.0871343728029249,-1.42129173458752E-5),.UNSPECIFIED.);
#1334=B_SPLINE_CURVE_WITH_KNOTS('',3,(#6193,#6194,#6195,#6196,#6197,#6198,
#6199,#6200,#6201,#6202,#6203,#6204,#6205,#6206),.UNSPECIFIED.,.F.,.F.,
(4,2,2,2,2,2,4),(1.00000006515879E-6,0.112920606874871,0.225073242572085,
0.350991141617053,0.476911503870067,0.589070561760002,0.701988545580405),
 .UNSPECIFIED.);
#1335=B_SPLINE_CURVE_WITH_KNOTS('',3,(#6207,#6208,#6209,#6210,#6211,#6212,
#6213,#6214,#6215,#6216,#6217,#6218,#6219,#6220),.UNSPECIFIED.,.F.,.F.,
(4,2,2,2,2,2,4),(-0.701988473605244,-0.589071180819017,-0.4769127850234,
-0.35099108445745,-0.225071862168092,-0.112919904371117,-1.00000006553191E-6),
 .UNSPECIFIED.);
#1336=B_SPLINE_CURVE_WITH_KNOTS('',3,(#6222,#6223,#6224,#6225,#6226,#6227,
#6228,#6229,#6230,#6231,#6232,#6233,#6234,#6235),.UNSPECIFIED.,.F.,.F.,
(4,2,2,2,2,2,4),(-0.701988434327251,-0.589071519766827,-0.476913463798924,
-0.350991050044857,-0.225071122030651,-0.112919515861704,-1.00000006708623E-6),
 .UNSPECIFIED.);
#1337=B_SPLINE_CURVE_WITH_KNOTS('',3,(#6236,#6237,#6238,#6239,#6240,#6241,
#6242,#6243,#6244,#6245,#6246,#6247,#6248,#6249),.UNSPECIFIED.,.F.,.F.,
(4,2,2,2,2,2,4),(1.00000006681659E-6,0.112920186660226,0.225072410288805,
0.350991103825395,0.476912269923873,0.589070928744561,0.701988502664996),
 .UNSPECIFIED.);
#1338=B_SPLINE_CURVE_WITH_KNOTS('',3,(#6251,#6252,#6253,#6254,#6255,#6256,
#6257,#6258,#6259,#6260,#6261,#6262,#6263,#6264),.UNSPECIFIED.,.F.,.F.,
(4,2,2,2,2,2,4),(1.00000006617394E-6,0.112919785545979,0.225071633871698,
0.350991068064418,0.476912983019837,0.589071278822759,0.701988461945112),
 .UNSPECIFIED.);
#1339=B_SPLINE_CURVE_WITH_KNOTS('',3,(#6265,#6266,#6267,#6268,#6269,#6270,
#6271,#6272,#6273,#6274,#6275,#6276,#6277,#6278),.UNSPECIFIED.,.F.,.F.,
(4,2,2,2,2,2,4),(-0.701988396950462,-0.589071843978261,-0.476914097866246,
-0.350991017380745,-0.225070429152157,-0.11291914402688,-1.00000006564294E-6),
 .UNSPECIFIED.);
#1340=B_SPLINE_CURVE_WITH_KNOTS('',3,(#6280,#6281,#6282,#6283,#6284,#6285,
#6286,#6287,#6288,#6289,#6290,#6291,#6292,#6293),.UNSPECIFIED.,.F.,.F.,
(4,2,2,2,2,2,4),(-0.701988361327658,-0.589072154539672,-0.476914691289198,
-0.350990986325078,-0.225069779289555,-0.112918787651099,-1.00000006719725E-6),
 .UNSPECIFIED.);
#1341=B_SPLINE_CURVE_WITH_KNOTS('',3,(#6294,#6295,#6296,#6297,#6298,#6299,
#6300,#6301,#6302,#6303,#6304,#6305,#6306,#6307),.UNSPECIFIED.,.F.,.F.,
(4,2,2,2,2,2,4),(1.00000006582091E-6,0.112919402052754,0.225070908050308,
0.350991034162431,0.476913648211992,0.589071613319107,0.701988423241176),
 .UNSPECIFIED.);
#1342=B_SPLINE_CURVE_WITH_KNOTS('',3,(#6309,#6310,#6311,#6312,#6313,#6314,
#6315,#6316,#6317,#6318,#6319,#6320,#6321,#6322),.UNSPECIFIED.,.F.,.F.,
(4,2,2,2,2,2,4),(1.0000000662017E-6,0.112919034863924,0.225070228189369,
0.350991001967214,0.476914269941965,0.589071933411044,0.701988386393479),
 .UNSPECIFIED.);
#1343=B_SPLINE_CURVE_WITH_KNOTS('',3,(#6323,#6324,#6325,#6326,#6327,#6328,
#6329,#6330,#6331,#6332,#6333,#6334,#6335,#6336),.UNSPECIFIED.,.F.,.F.,
(4,2,2,2,2,2,4),(-0.701988327327066,-0.589072452423603,-0.47691524766257,
-0.350990956752978,-0.225069168686889,-0.112918445645089,-1.00000006486578E-6),
 .UNSPECIFIED.);
#1344=B_SPLINE_CURVE_WITH_KNOTS('',3,(#6338,#6339,#6340,#6341,#6342,#6343,
#6344,#6345,#6346,#6347,#6348,#6349,#6350,#6351),.UNSPECIFIED.,.F.,.F.,
(4,2,2,2,2,2,4),(-0.701988294830502,-0.589072738504006,-0.476915770177297,
-0.350990928552615,-0.225068594007581,-0.112918117029042,-1.00000006530987E-6),
 .UNSPECIFIED.);
#1345=B_SPLINE_CURVE_WITH_KNOTS('',3,(#6352,#6353,#6354,#6355,#6356,#6357,
#6358,#6359,#6360,#6361,#6362,#6363,#6364,#6365),.UNSPECIFIED.,.F.,.F.,
(4,2,2,2,2,2,4),(1.00000006624442E-6,0.112918682802859,0.225069590196386,
0.350990971343344,0.476914852128502,0.589072240149847,0.701988351259665),
 .UNSPECIFIED.);
#1346=B_SPLINE_CURVE_WITH_KNOTS('',3,(#6367,#6368,#6369,#6370,#6371,#6372,
#6373,#6374,#6375,#6376,#6377,#6378,#6379,#6380),.UNSPECIFIED.,.F.,.F.,
(4,2,2,2,2,2,4),(1.00000006535993E-6,0.112918344813946,0.225068990444782,
0.350990942169864,0.476915398241522,0.589072534477526,0.701988317711996),
 .UNSPECIFIED.);
#1347=B_SPLINE_CURVE_WITH_KNOTS('',3,(#6381,#6382,#6383,#6384,#6385,#6386,
#6387,#6388,#6389,#6390,#6391,#6392,#6393,#6394),.UNSPECIFIED.,.F.,.F.,
(4,2,2,2,2,2,4),(-0.70198826373142,-0.589073013568951,-0.476916261675244,
-0.350990901623609,-0.225068052277895,-0.112917800918598,-1.00000006786338E-6),
 .UNSPECIFIED.);
#1348=B_SPLINE_CURVE_WITH_KNOTS('',3,(#6396,#6397,#6398,#6399,#6400,#6401,
#6402,#6403,#6404,#6405,#6406,#6407,#6408,#6409),.UNSPECIFIED.,.F.,.F.,
(4,2,2,2,2,2,4),(-0.701988233933622,-0.589073278331429,-0.476916724695184,
-0.350990875875406,-0.225067540839014,-0.112917496512839,-1.0000000669752E-6),
 .UNSPECIFIED.);
#1349=B_SPLINE_CURVE_WITH_KNOTS('',3,(#6410,#6411,#6412,#6413,#6414,#6415,
#6416,#6417,#6418,#6419,#6420,#6421,#6422,#6423),.UNSPECIFIED.,.F.,.F.,
(4,2,2,2,2,2,4),(1.00000006543456E-6,0.112918019946688,0.225068425709767,
0.35099091433838,0.476915911364266,0.589072817241646,0.701988285635971),
 .UNSPECIFIED.);
#1350=B_SPLINE_CURVE_WITH_KNOTS('',3,(#6425,#6426,#6427,#6428,#6429,#6430,
#6431,#6432,#6433,#6434,#6435,#6436,#6437,#6438),.UNSPECIFIED.,.F.,.F.,
(4,2,2,2,2,2,4),(1.00000006721342E-6,0.112917707342306,0.225067893114481,
0.350990887751436,0.476916394245156,0.589073089207131,0.701988254928176),
 .UNSPECIFIED.);
#1351=B_SPLINE_CURVE_WITH_KNOTS('',3,(#6439,#6440,#6441,#6442,#6443,#6444,
#6445,#6446,#6447,#6448,#6449,#6450,#6451,#6452),.UNSPECIFIED.,.F.,.F.,
(4,2,2,2,2,2,4),(-0.701988205350069,-0.589073533438657,-0.476917161512005,
-0.350990851226291,-0.225067057306856,-0.112917203084259,-1.00000006542089E-6),
 .UNSPECIFIED.);
#1352=B_SPLINE_CURVE_WITH_KNOTS('',3,(#6454,#6455,#6456,#6457,#6458,#6459,
#6460,#6461,#6462,#6463,#6464,#6465,#6466,#6467),.UNSPECIFIED.,.F.,.F.,
(4,2,2,2,2,2,4),(-0.701988177901583,-0.589073779479684,-0.476917574169643,
-0.35099082760215,-0.225066599537539,-0.112916919970041,-1.00000006586498E-6),
 .UNSPECIFIED.);
#1353=B_SPLINE_CURVE_WITH_KNOTS('',3,(#6468,#6469,#6470,#6471,#6472,#6473,
#6474,#6475,#6476,#6477,#6478,#6479,#6480,#6481),.UNSPECIFIED.,.F.,.F.,
(4,2,2,2,2,2,4),(1.0000000653107E-6,0.112917406222399,0.225067390084615,
0.35099086232123,0.476916849341858,0.589073351066865,0.701988225495295),
 .UNSPECIFIED.);
#1354=B_SPLINE_CURVE_WITH_KNOTS('',3,(#6483,#6484,#6485,#6486,#6487,#6488,
#6489,#6490,#6491,#6492,#6493,#6494,#6495,#6496),.UNSPECIFIED.,.F.,.F.,
(4,2,2,2,2,2,4),(1.00000006686074E-6,0.112917115879217,0.22506691430973,
0.35099083796823,0.476917278858146,0.589073603450107,0.701988197252594),
 .UNSPECIFIED.);
#1355=B_SPLINE_CURVE_WITH_KNOTS('',3,(#6497,#6498,#6499,#6500,#6501,#6502,
#6503,#6504,#6505,#6506,#6507,#6508,#6509,#6510),.UNSPECIFIED.,.F.,.F.,
(4,2,2,2,2,2,4),(-0.701988151516124,-0.589074016992278,-0.476917964509549,
-0.350990804935719,-0.225066165598174,-0.11291664656469,-1.00000006575396E-6),
 .UNSPECIFIED.);
#1356=B_SPLINE_CURVE_WITH_KNOTS('',3,(#6512,#6513,#6514,#6515,#6516,#6517,
#6518,#6519,#6520,#6521,#6522,#6523,#6524,#6525),.UNSPECIFIED.,.F.,.F.,
(4,2,2,2,2,2,4),(-0.701988126127907,-0.589074246468584,-0.476918334194806,
-0.350990783165686,-0.225065753741602,-0.112916382313578,-1.000000065976E-6),
 .UNSPECIFIED.);
#1357=B_SPLINE_CURVE_WITH_KNOTS('',3,(#6526,#6527,#6528,#6529,#6530,#6531,
#6532,#6533,#6534,#6535,#6536,#6537,#6538,#6539),.UNSPECIFIED.,.F.,.F.,
(4,2,2,2,2,2,4),(1.00000006463131E-6,0.112916835667461,0.225066463710663,
0.350990814620418,0.476917684775841,0.589073846930262,0.701988170123163),
 .UNSPECIFIED.);
#1358=B_SPLINE_CURVE_WITH_KNOTS('',3,(#6542,#6543,#6544,#6545,#6546,#6547,
#6548,#6549,#6550,#6551,#6552,#6553,#6554,#6555),.UNSPECIFIED.,.F.,.F.,
(4,2,2,2,2,2,4),(3.23003133540915E-5,0.0747831774093426,0.149363713796628,
0.275774683581478,0.338728441304644,0.44478522977372,0.551343968794629),
 .UNSPECIFIED.);
#1359=B_SPLINE_CURVE_WITH_KNOTS('',3,(#6558,#6559,#6560,#6561,#6562,#6563),
 .UNSPECIFIED.,.F.,.F.,(4,2,4),(-0.150154722490422,-0.0750773651805342,
0.),.UNSPECIFIED.);
#1360=B_SPLINE_CURVE_WITH_KNOTS('',3,(#6581,#6582,#6583,#6584),
 .UNSPECIFIED.,.F.,.F.,(4,4),(0.,0.349249092707648),.UNSPECIFIED.);
#1361=B_SPLINE_CURVE_WITH_KNOTS('',3,(#6611,#6612,#6613,#6614,#6615,#6616,
#6617,#6618,#6619,#6620,#6621,#6622,#6623,#6624,#6625,#6626,#6627,#6628,
#6629,#6630,#6631,#6632,#6633,#6634,#6635,#6636,#6637,#6638,#6639,#6640,
#6641,#6642,#6643,#6644,#6645,#6646,#6647,#6648,#6649,#6650,#6651,#6652,
#6653,#6654,#6655,#6656,#6657,#6658,#6659),.UNSPECIFIED.,.F.,.F.,(4,3,3,
3,3,3,3,3,3,3,3,3,3,3,3,3,4),(0.,0.036532739404764,0.0731538029882342,0.109091393921472,
0.133009526612987,0.146488998525985,0.154769879434264,0.190069930149183,
0.204763924687531,0.240416666524628,0.275945870858501,0.295512148258635,
0.303306009056309,0.338041865699653,0.372454604100603,0.40666751045333,
0.414264078313279),.UNSPECIFIED.);
#1362=B_SPLINE_CURVE_WITH_KNOTS('',3,(#6660,#6661,#6662,#6663,#6664),
 .UNSPECIFIED.,.F.,.F.,(4,1,4),(39.5699522859152,40.0185665844411,40.2123850074524),
 .UNSPECIFIED.);
#1363=B_SPLINE_CURVE_WITH_KNOTS('',3,(#6689,#6690,#6691,#6692,#6693,#6694),
 .UNSPECIFIED.,.F.,.F.,(4,1,1,4),(33.2867669787356,33.7353812772616,34.4581548699468,
34.9067691684727),.UNSPECIFIED.);
#1364=B_SPLINE_CURVE_WITH_KNOTS('',3,(#6719,#6720,#6721,#6722,#6723,#6724),
 .UNSPECIFIED.,.F.,.F.,(4,1,1,4),(27.003581671556,27.452195970082,28.1749695627672,
28.6235838612931),.UNSPECIFIED.);
#1365=B_SPLINE_CURVE_WITH_KNOTS('',3,(#6749,#6750,#6751,#6752,#6753,#6754),
 .UNSPECIFIED.,.F.,.F.,(4,1,1,4),(20.7203963643765,21.1690106629024,21.8917842555876,
22.3403985541136),.UNSPECIFIED.);
#1366=B_SPLINE_CURVE_WITH_KNOTS('',3,(#6779,#6780,#6781,#6782,#6783,#6784),
 .UNSPECIFIED.,.F.,.F.,(4,1,1,4),(14.4372110571969,14.8858253557228,15.608598948408,
16.057213246934),.UNSPECIFIED.);
#1367=B_SPLINE_CURVE_WITH_KNOTS('',3,(#6809,#6810,#6811,#6812,#6813,#6814),
 .UNSPECIFIED.,.F.,.F.,(4,1,1,4),(8.15402575001729,8.60264004854321,9.32541364122847,
9.77402793975438),.UNSPECIFIED.);
#1368=B_SPLINE_CURVE_WITH_KNOTS('',3,(#6839,#6840,#6841,#6842,#6843,#6844,
#6845,#6846,#6847,#6848,#6849,#6850,#6851,#6852,#6853,#6854,#6855,#6856,
#6857,#6858,#6859,#6860,#6861,#6862,#6863,#6864,#6865,#6866,#6867,#6868,
#6869,#6870,#6871,#6872,#6873,#6874,#6875,#6876,#6877,#6878,#6879,#6880,
#6881,#6882,#6883,#6884,#6885,#6886,#6887,#6888,#6889,#6890,#6891,#6892,
#6893,#6894,#6895,#6896,#6897,#6898,#6899,#6900,#6901,#6902,#6903,#6904,
#6905),.UNSPECIFIED.,.F.,.F.,(4,3,3,3,3,3,3,3,3,3,3,3,3,3,3,3,3,3,3,3,3,
3,4),(1.87084198259956,1.99926342031853,2.05566622969097,2.13790680565216,
2.14812754057612,2.24061018839636,2.33315480194847,2.36709157385711,2.36709841394138,
2.45784756460922,2.54854382431794,2.63920461494343,2.72984732525151,2.82051706645472,
2.91119807753201,3.00194817584722,3.06604332828347,3.06605017033776,3.1596597536536,
3.2532033890349,3.34670011823176,3.48217495951514,3.49084263257479),
 .UNSPECIFIED.);
#1369=B_SPLINE_CURVE_WITH_KNOTS('',3,(#6931,#6932,#6933,#6934,#6935,#6936),
 .UNSPECIFIED.,.F.,.F.,(4,1,1,4),(36.4283596323254,36.8769739308513,37.5997475235366,
38.0483618220625),.UNSPECIFIED.);
#1370=B_SPLINE_CURVE_WITH_KNOTS('',3,(#6961,#6962,#6963,#6964,#6965,#6966),
 .UNSPECIFIED.,.F.,.F.,(4,1,1,4),(30.1451743251458,30.5937886236718,31.316562216357,
31.7651765148829),.UNSPECIFIED.);
#1371=B_SPLINE_CURVE_WITH_KNOTS('',3,(#6991,#6992,#6993,#6994,#6995,#6996),
 .UNSPECIFIED.,.F.,.F.,(4,1,1,4),(23.8619890179663,24.3106033164922,25.0333769091774,
25.4819912077033),.UNSPECIFIED.);
#1372=B_SPLINE_CURVE_WITH_KNOTS('',3,(#7021,#7022,#7023,#7024,#7025,#7026),
 .UNSPECIFIED.,.F.,.F.,(4,1,1,4),(17.5788037107867,18.0274180093126,18.7501916019978,
19.1988059005238),.UNSPECIFIED.);
#1373=B_SPLINE_CURVE_WITH_KNOTS('',3,(#7051,#7052,#7053,#7054,#7055,#7056),
 .UNSPECIFIED.,.F.,.F.,(4,1,1,4),(11.2956184036071,11.744232702133,12.4670062948183,
12.9156205933442),.UNSPECIFIED.);
#1374=B_SPLINE_CURVE_WITH_KNOTS('',3,(#7081,#7082,#7083,#7084,#7085,#7086),
 .UNSPECIFIED.,.F.,.F.,(4,1,1,4),(5.0124330964275,5.46104739495341,6.18382098763867,
6.63243528616458),.UNSPECIFIED.);
#1375=B_SPLINE_CURVE_WITH_KNOTS('',3,(#7088,#7089,#7090,#7091,#7092,#7093,
#7094,#7095,#7096,#7097,#7098,#7099,#7100,#7101,#7102,#7103,#7104,#7105,
#7106,#7107,#7108,#7109,#7110,#7111,#7112,#7113,#7114,#7115,#7116,#7117,
#7118,#7119,#7120,#7121,#7122,#7123,#7124,#7125,#7126,#7127,#7128,#7129,
#7130),.UNSPECIFIED.,.F.,.F.,(4,3,3,3,3,3,3,3,3,3,3,3,3,3,4),(4.96552804228439E-5,
0.0320183427279736,0.0643403602042524,0.0886933568687708,0.117718239582565,
0.124682181362639,0.131745609822757,0.164253554234894,0.197241305764055,
0.230517869072714,0.25235595445092,0.259992045647903,0.264659623072051,
0.298823823008935,0.320892418579125),.UNSPECIFIED.);
#1376=B_SPLINE_CURVE_WITH_KNOTS('',3,(#7135,#7136,#7137,#7138,#7139,#7140),
 .UNSPECIFIED.,.F.,.F.,(4,1,1,4),(-3.33195380826789,-2.88333950974197,-2.16056591705671,
-2.06120159751576),.UNSPECIFIED.);
#1377=B_SPLINE_CURVE_WITH_KNOTS('',3,(#7143,#7144,#7145,#7146,#7147,#7148,
#7149,#7150,#7151,#7152,#7153,#7154,#7155,#7156,#7157,#7158,#7159,#7160,
#7161,#7162,#7163,#7164,#7165,#7166,#7167,#7168,#7169,#7170,#7171,#7172,
#7173,#7174,#7175,#7176,#7177,#7178,#7179,#7180,#7181,#7182,#7183,#7184,
#7185,#7186,#7187,#7188,#7189,#7190,#7191,#7192,#7193,#7194,#7195,#7196,
#7197,#7198,#7199,#7200,#7201,#7202,#7203),.UNSPECIFIED.,.F.,.F.,(4,3,3,
3,3,3,3,3,3,3,3,3,3,3,3,3,3,3,3,3,4),(-41.0310632895362,-40.9388473190672,
-40.7871353339006,-40.754407737536,-40.6621654402305,-40.5698612720643,
-40.4813329034246,-40.4813266946942,-40.3903969656387,-40.2995162802569,
-40.2086677147606,-40.1178343757824,-40.0269750194882,-39.9361025632024,
-39.8451701195949,-39.8091216443534,-39.8091154310716,-39.7151490717192,
-39.6212411951498,-39.5273766833117,-39.4110634616083),.UNSPECIFIED.);
#1378=B_SPLINE_CURVE_WITH_KNOTS('',3,(#7205,#7206,#7207,#7208,#7209,#7210),
 .UNSPECIFIED.,.F.,.F.,(4,1,1,4),(-37.8894729977556,-37.4408586992297,-36.7180851065444,
-36.2694708080185),.UNSPECIFIED.);
#1379=B_SPLINE_CURVE_WITH_KNOTS('',3,(#7212,#7213,#7214,#7215,#7216,#7217),
 .UNSPECIFIED.,.F.,.F.,(4,1,1,4),(-34.7478803441658,-34.2992660456399,-33.5764924529546,
-33.1278781544287),.UNSPECIFIED.);
#1380=B_SPLINE_CURVE_WITH_KNOTS('',3,(#7219,#7220,#7221,#7222,#7223,#7224),
 .UNSPECIFIED.,.F.,.F.,(4,1,1,4),(-31.606287690576,-31.1576733920501,-30.4348997993648,
-29.9862855008389),.UNSPECIFIED.);
#1381=B_SPLINE_CURVE_WITH_KNOTS('',3,(#7226,#7227,#7228,#7229,#7230,#7231),
 .UNSPECIFIED.,.F.,.F.,(4,1,1,4),(-28.4646950369862,-28.0160807384603,-27.2933071457751,
-26.8446928472491),.UNSPECIFIED.);
#1382=B_SPLINE_CURVE_WITH_KNOTS('',3,(#7233,#7234,#7235,#7236,#7237,#7238),
 .UNSPECIFIED.,.F.,.F.,(4,1,1,4),(-25.3231023833964,-24.8744880848705,-24.1517144921853,
-23.7031001936593),.UNSPECIFIED.);
#1383=B_SPLINE_CURVE_WITH_KNOTS('',3,(#7240,#7241,#7242,#7243,#7244,#7245),
 .UNSPECIFIED.,.F.,.F.,(4,1,1,4),(-22.1815097298066,-21.7328954312807,-21.0101218385955,
-20.5615075400696),.UNSPECIFIED.);
#1384=B_SPLINE_CURVE_WITH_KNOTS('',3,(#7247,#7248,#7249,#7250,#7251,#7252),
 .UNSPECIFIED.,.F.,.F.,(4,1,1,4),(-19.0399170762168,-18.5913027776909,-17.8685291850057,
-17.4199148864798),.UNSPECIFIED.);
#1385=B_SPLINE_CURVE_WITH_KNOTS('',3,(#7254,#7255,#7256,#7257,#7258,#7259),
 .UNSPECIFIED.,.F.,.F.,(4,1,1,4),(-15.8983244226271,-15.4497101241011,-14.7269365314159,
-14.27832223289),.UNSPECIFIED.);
#1386=B_SPLINE_CURVE_WITH_KNOTS('',3,(#7261,#7262,#7263,#7264,#7265,#7266),
 .UNSPECIFIED.,.F.,.F.,(4,1,1,4),(-12.7567317690373,-12.3081174705113,-11.5853438778261,
-11.1367295793002),.UNSPECIFIED.);
#1387=B_SPLINE_CURVE_WITH_KNOTS('',3,(#7268,#7269,#7270,#7271,#7272,#7273),
 .UNSPECIFIED.,.F.,.F.,(4,1,1,4),(-9.61513911544747,-9.16652481692155,-8.4437512242363,
-7.99513692571038),.UNSPECIFIED.);
#1388=B_SPLINE_CURVE_WITH_KNOTS('',3,(#7275,#7276,#7277,#7278,#7279,#7280),
 .UNSPECIFIED.,.F.,.F.,(4,1,1,4),(-6.47354646185768,-6.02493216333176,-5.3021585706465,
-4.85354427212059),.UNSPECIFIED.);
#1389=B_SPLINE_CURVE_WITH_KNOTS('',3,(#7610,#7611,#7612,#7613,#7614,#7615),
 .UNSPECIFIED.,.F.,.F.,(4,2,4),(-0.130044971937413,-0.0647221669300852,
0.),.UNSPECIFIED.);
#1390=B_SPLINE_CURVE_WITH_KNOTS('',3,(#7647,#7648,#7649,#7650,#7651,#7652,
#7653,#7654,#7655,#7656,#7657,#7658,#7659,#7660,#7661,#7662,#7663,#7664,
#7665,#7666,#7667,#7668,#7669,#7670,#7671,#7672,#7673,#7674,#7675,#7676,
#7677,#7678,#7679,#7680,#7681,#7682,#7683,#7684,#7685,#7686,#7687,#7688,
#7689,#7690,#7691,#7692,#7693,#7694,#7695,#7696,#7697,#7698,#7699,#7700,
#7701,#7702,#7703,#7704,#7705,#7706,#7707,#7708,#7709,#7710,#7711,#7712,
#7713,#7714,#7715,#7716,#7717,#7718,#7719,#7720,#7721,#7722,#7723,#7724,
#7725,#7726,#7727,#7728,#7729,#7730,#7731,#7732,#7733,#7734,#7735,#7736,
#7737,#7738,#7739,#7740,#7741,#7742,#7743,#7744,#7745,#7746,#7747,#7748,
#7749,#7750,#7751,#7752,#7753,#7754,#7755,#7756,#7757,#7758,#7759,#7760,
#7761,#7762,#7763,#7764,#7765,#7766,#7767,#7768,#7769,#7770,#7771,#7772,
#7773,#7774,#7775,#7776,#7777,#7778,#7779,#7780,#7781,#7782,#7783,#7784,
#7785,#7786,#7787,#7788,#7789,#7790,#7791,#7792,#7793,#7794,#7795,#7796,
#7797,#7798,#7799,#7800,#7801,#7802,#7803,#7804,#7805,#7806,#7807,#7808,
#7809,#7810,#7811,#7812,#7813,#7814,#7815,#7816,#7817,#7818,#7819,#7820,
#7821,#7822,#7823,#7824,#7825,#7826,#7827,#7828,#7829,#7830,#7831,#7832,
#7833),.UNSPECIFIED.,.F.,.F.,(4,3,3,3,3,3,3,3,3,3,3,3,3,3,3,3,3,3,3,3,3,
3,3,3,3,3,3,3,3,3,3,3,3,3,3,3,3,3,3,3,3,3,3,3,3,3,3,3,3,3,3,3,3,3,3,3,3,
3,3,3,3,3,4),(10.3850888958016,10.4641373814769,10.5520588327897,10.6410762182378,
10.7288594652779,10.8166179102709,10.9043752172213,10.9943308920096,11.0822044534747,
11.1676514039115,11.1732011849246,11.2524595516301,11.2641583632187,11.2641979163745,
11.3459974247077,11.3543883418031,11.4444664958327,11.5344565843787,11.6243852832326,
11.7142815564214,11.804167167181,11.8940638650899,11.9840486455302,12.074077267802,
12.1642488110667,12.2472698528716,12.247304603897,12.3294279854305,12.337349377077,
12.4272819895897,12.517126854226,12.6069114553117,12.6966643802678,12.786407578033,
12.8761629846047,12.9660091578037,13.0559004439681,13.1459382866182,13.2303745458392,
13.2304112914194,13.3122318951338,13.3202803122904,13.4100337681398,13.4996963272619,
13.5892945887802,13.6788587810357,13.7684110716423,13.8579736136466,13.947625011734,
14.0373201915803,14.1271617222868,14.2075665015184,14.2134811498394,14.2135179789419,
14.2954243505238,14.3034962162208,14.3933692649306,14.4831592957879,14.5728884092593,
14.6625930287075,14.7522802792272,14.8420075718479,14.9177889943201),
 .UNSPECIFIED.);
#1391=B_SPLINE_CURVE_WITH_KNOTS('',3,(#7836,#7837,#7838,#7839,#7840,#7841,
#7842,#7843,#7844,#7845,#7846,#7847,#7848,#7849,#7850,#7851,#7852,#7853,
#7854,#7855,#7856,#7857,#7858,#7859,#7860,#7861,#7862,#7863,#7864,#7865,
#7866,#7867,#7868,#7869,#7870,#7871,#7872,#7873,#7874,#7875,#7876,#7877,
#7878,#7879,#7880,#7881,#7882,#7883,#7884,#7885,#7886,#7887,#7888,#7889,
#7890,#7891,#7892,#7893,#7894,#7895,#7896,#7897,#7898,#7899,#7900,#7901,
#7902,#7903,#7904,#7905,#7906,#7907,#7908,#7909,#7910,#7911,#7912,#7913,
#7914,#7915,#7916,#7917,#7918,#7919,#7920,#7921,#7922,#7923,#7924,#7925,
#7926,#7927,#7928,#7929,#7930,#7931,#7932,#7933,#7934,#7935,#7936,#7937,
#7938,#7939,#7940,#7941,#7942,#7943,#7944,#7945,#7946,#7947,#7948,#7949,
#7950,#7951,#7952,#7953,#7954,#7955,#7956,#7957,#7958,#7959,#7960,#7961,
#7962,#7963,#7964,#7965,#7966,#7967,#7968,#7969,#7970,#7971),
 .UNSPECIFIED.,.F.,.F.,(4,3,3,3,3,3,3,3,3,3,3,3,3,3,3,3,3,3,3,3,3,3,3,3,
3,3,3,3,3,3,3,3,3,3,3,3,3,3,3,3,3,3,3,3,3,4),(11.6150691238056,11.716887748291,
11.818807396451,11.9206982029579,12.0224123053014,12.106615918772,12.1066224675668,
12.1974625342849,12.2882944241597,12.379171523673,12.4700739203339,12.561061507472,
12.598175811328,12.5981975387223,12.6813394695241,12.6891753523971,12.7800935403341,
12.8709528368157,12.9617902529354,13.0526187338464,13.1434585576012,13.2343300061399,
13.3253148905754,13.4163587789532,13.5075598865992,13.5812824988505,13.5813185969407,
13.66123779196,13.6704071444793,13.7594059294644,13.8483044456942,13.9378150382791,
14.0265967435875,14.1153607025908,14.2041298440541,14.2941946796338,14.3830904507549,
14.4737398185639,14.5549025675923,14.5643891863729,14.5644292218501,14.6449085802043,
14.6545593024114,14.7446311850219,14.8346130791444,14.9185733201878),
 .UNSPECIFIED.);
#1392=B_SPLINE_CURVE_WITH_KNOTS('',3,(#7976,#7977,#7978,#7979,#7980,#7981,
#7982,#7983,#7984,#7985,#7986,#7987,#7988,#7989,#7990,#7991,#7992,#7993,
#7994,#7995,#7996,#7997,#7998,#7999,#8000,#8001,#8002,#8003,#8004,#8005,
#8006,#8007,#8008,#8009,#8010,#8011,#8012,#8013,#8014,#8015,#8016,#8017,
#8018,#8019,#8020,#8021,#8022,#8023,#8024,#8025,#8026,#8027,#8028,#8029,
#8030,#8031,#8032,#8033,#8034,#8035,#8036,#8037,#8038,#8039,#8040,#8041,
#8042,#8043,#8044,#8045,#8046,#8047,#8048,#8049,#8050,#8051,#8052,#8053,
#8054,#8055,#8056,#8057,#8058,#8059,#8060,#8061,#8062,#8063,#8064,#8065,
#8066,#8067,#8068,#8069,#8070,#8071,#8072,#8073,#8074,#8075,#8076,#8077,
#8078,#8079,#8080,#8081,#8082,#8083,#8084,#8085,#8086,#8087,#8088,#8089,
#8090,#8091,#8092,#8093,#8094,#8095,#8096,#8097,#8098,#8099,#8100,#8101,
#8102,#8103,#8104,#8105,#8106,#8107,#8108,#8109,#8110,#8111,#8112,#8113,
#8114,#8115,#8116,#8117,#8118,#8119,#8120,#8121,#8122,#8123,#8124,#8125,
#8126,#8127,#8128,#8129,#8130,#8131,#8132,#8133,#8134,#8135,#8136,#8137,
#8138,#8139,#8140,#8141,#8142,#8143,#8144,#8145,#8146,#8147),
 .UNSPECIFIED.,.F.,.F.,(4,2,2,2,2,2,2,2,2,2,2,2,2,2,2,2,2,2,2,2,2,2,2,2,
2,2,2,2,2,2,2,2,2,2,2,2,2,2,2,2,2,2,2,2,2,2,2,2,2,2,2,2,2,2,2,2,2,2,2,2,
2,2,2,2,2,2,2,2,2,2,2,2,2,2,2,2,2,2,2,2,2,2,2,2,2,4),(-2.34349935747219,
-2.32479321244631,-2.3115095086961,-2.30353059275682,-2.29532108129983,
-2.28088936810031,-2.26189886696644,-2.20929781208258,-2.15450652873946,
-2.13394329508488,-2.12155686493844,-2.10788626489361,-2.08783834376536,
-2.03424657964964,-1.95860390922288,-1.94507668101036,-1.93704913924088,
-1.92889606131535,-1.91474449864053,-1.89626288592835,-1.84654371676776,
-1.78804151246791,-1.76738860818391,-1.75361468301218,-1.73969844149924,
-1.71824200221813,-1.69214031600218,-1.62636836462047,-1.58789145006146,
-1.57643226148622,-1.56877805451772,-1.55996076245785,-1.54234252694852,
-1.51710804433584,-1.47285455929373,-1.42093470919277,-1.40050503777244,
-1.38814022198954,-1.37444924313941,-1.35427615186781,-1.30006083507845,
-1.22569587408321,-1.21196384643384,-1.2038950116354,-1.19578131764764,
-1.18183742260512,-1.13378381169967,-1.05260288386253,-1.03294463075192,
-1.01947068923136,-1.00535317643753,-0.982805291875028,-0.921353089151828,
-0.858204884788433,-0.844923691725052,-0.836944277344367,-0.828737610032856,
-0.81430811178137,-0.795319608194366,-0.742722325438803,-0.687907248193089,
-0.667347214427635,-0.654966036493293,-0.641304419454002,-0.621277994696126,
-0.567810711042773,-0.491908125022253,-0.47842388550636,-0.470408074913927,
-0.462255044052201,-0.448086925837385,-0.429574435509035,-0.379697817459574,
-0.321252544528174,-0.300590533312429,-0.286816292445277,-0.27290500586233,
-0.251468064151761,-0.225396140987684,-0.159778836579698,-0.121158200649779,
-0.109685408742185,-0.102018673693576,-0.0931614321386275,-0.0754292161435672,
-0.000158205331122453),.UNSPECIFIED.);
#1393=B_SPLINE_CURVE_WITH_KNOTS('',3,(#8148,#8149,#8150,#8151,#8152,#8153,
#8154,#8155,#8156,#8157,#8158,#8159,#8160,#8161,#8162,#8163,#8164,#8165,
#8166,#8167,#8168,#8169,#8170,#8171,#8172,#8173,#8174,#8175,#8176,#8177,
#8178,#8179,#8180,#8181,#8182,#8183,#8184,#8185,#8186,#8187,#8188,#8189,
#8190,#8191,#8192,#8193,#8194,#8195,#8196,#8197,#8198,#8199,#8200,#8201,
#8202,#8203,#8204,#8205,#8206,#8207,#8208,#8209,#8210,#8211,#8212,#8213,
#8214,#8215,#8216,#8217,#8218,#8219,#8220,#8221,#8222,#8223,#8224,#8225,
#8226,#8227,#8228,#8229,#8230,#8231,#8232,#8233,#8234,#8235,#8236,#8237,
#8238,#8239,#8240,#8241,#8242,#8243,#8244,#8245,#8246,#8247,#8248,#8249,
#8250,#8251,#8252,#8253,#8254,#8255,#8256,#8257,#8258,#8259,#8260,#8261,
#8262,#8263,#8264,#8265,#8266,#8267,#8268,#8269,#8270,#8271,#8272,#8273,
#8274,#8275,#8276,#8277,#8278,#8279,#8280,#8281,#8282,#8283,#8284,#8285,
#8286,#8287,#8288,#8289,#8290,#8291,#8292,#8293,#8294,#8295,#8296,#8297,
#8298,#8299,#8300,#8301,#8302,#8303,#8304,#8305,#8306,#8307,#8308,#8309,
#8310,#8311,#8312,#8313,#8314,#8315),.UNSPECIFIED.,.F.,.F.,(4,2,2,2,2,2,
2,2,2,2,2,2,2,2,2,2,2,2,2,2,2,2,2,2,2,2,2,2,2,2,2,2,2,2,2,2,2,2,2,2,2,2,
2,2,2,2,2,2,2,2,2,2,2,2,2,2,2,2,2,2,2,2,2,2,2,2,2,2,2,2,2,2,2,2,2,2,2,2,
2,2,2,2,2,4),(-12.0121045471319,-11.9908765110274,-11.9746552288482,-11.9620401761327,
-11.9485323873418,-11.9311366610153,-11.8881357893894,-11.8073824176125,
-11.7892270360545,-11.7801851308519,-11.772439210027,-11.7608113343547,
-11.7188325800486,-11.6562211330763,-11.6307170509891,-11.6096421761874,
-11.5958396202625,-11.5820863501214,-11.5612988389604,-11.4917675903954,
-11.4492693879947,-11.4322152629272,-11.4188825625983,-11.4109381992301,
-11.4028732288876,-11.3889027591304,-11.3361610911638,-11.2654114051204,
-11.2430699259675,-11.2290912255745,-11.215769797557,-11.1963964587597,
-11.1134640302362,-11.0662228114669,-11.0524250800485,-11.0443936055418,
-11.0363673713181,-11.0227534785367,-10.9629834042421,-10.9148133988729,
-10.8922381306211,-10.8729136314128,-10.8593852164036,-10.8451946670713,
-10.8221064791139,-10.7287784010119,-10.7051397925194,-10.6883037169419,
-10.679635851479,-10.6720470804712,-10.66039924893,-10.6164842479188,-10.5373715822647,
-10.512352604061,-10.4978361838047,-10.4845081137113,-10.4663250505177,
-10.4114707069489,-10.3547296673,-10.3350754146237,-10.3202982198305,-10.3120482621597,
-10.3041857562166,-10.2913544933126,-10.2231672905296,-10.1654515082249,
-10.1432424285699,-10.1292419722719,-10.1158244545399,-10.0961572061151,
-10.015350938565,-9.97964995117286,-9.96415391429196,-9.95172596416459,
-9.94393776729407,-9.93556012340714,-9.9201582013566,-9.85052325946428,
-9.79061306498618,-9.77224860026096,-9.75888936619271,-9.74443089117664,
-9.71976128169862,-9.66952787558574),.UNSPECIFIED.);
#1394=B_SPLINE_CURVE_WITH_KNOTS('',3,(#8320,#8321,#8322,#8323,#8324,#8325,
#8326,#8327,#8328,#8329,#8330,#8331,#8332,#8333,#8334,#8335,#8336,#8337,
#8338,#8339,#8340,#8341,#8342,#8343,#8344,#8345,#8346,#8347,#8348,#8349,
#8350,#8351,#8352,#8353,#8354,#8355,#8356,#8357,#8358,#8359,#8360,#8361,
#8362,#8363,#8364,#8365,#8366,#8367,#8368,#8369,#8370,#8371,#8372,#8373,
#8374,#8375,#8376,#8377,#8378,#8379,#8380,#8381,#8382,#8383,#8384,#8385,
#8386,#8387,#8388,#8389,#8390,#8391,#8392,#8393,#8394,#8395,#8396,#8397,
#8398,#8399,#8400,#8401,#8402,#8403,#8404,#8405,#8406,#8407,#8408,#8409,
#8410,#8411,#8412,#8413,#8414,#8415,#8416,#8417,#8418,#8419,#8420,#8421,
#8422,#8423,#8424,#8425,#8426,#8427,#8428,#8429,#8430,#8431,#8432,#8433,
#8434,#8435,#8436,#8437,#8438,#8439,#8440,#8441,#8442,#8443,#8444,#8445,
#8446,#8447,#8448,#8449,#8450,#8451,#8452,#8453,#8454,#8455,#8456,#8457,
#8458,#8459,#8460,#8461,#8462,#8463,#8464,#8465,#8466,#8467,#8468,#8469,
#8470,#8471,#8472,#8473,#8474,#8475,#8476,#8477,#8478,#8479,#8480,#8481,
#8482,#8483,#8484,#8485),.UNSPECIFIED.,.F.,.F.,(4,2,2,2,2,2,2,2,2,2,2,2,
2,2,2,2,2,2,2,2,2,2,2,2,2,2,2,2,2,2,2,2,2,2,2,2,2,2,2,2,2,2,2,2,2,2,2,2,
2,2,2,2,2,2,2,2,2,2,2,2,2,2,2,2,2,2,2,2,2,2,2,2,2,2,2,2,2,2,2,2,2,2,4),
(-4.6872551568627,-4.68453856924504,-4.66991807190972,-4.64460086592956,
-4.56421223924462,-4.52178108697756,-4.51014758765552,-4.50254083643499,
-4.49383144259538,-4.47681210054929,-4.45282204631766,-4.40676877106719,
-4.35448822173273,-4.33403881478831,-4.321668850125,-4.30797717731899,-4.28781372718408,
-4.26388279683943,-4.20976031928825,-4.15941791454452,-4.14557393886306,
-4.13748201867114,-4.1293941168964,-4.11557044478061,-4.0685869812435,-3.98550638224759,
-3.96609140230899,-3.95265842757976,-3.93848031642065,-3.91558953360281,
-3.86196741561931,-3.79000665350435,-3.77756736530792,-3.77051785566562,
-3.76235952107894,-3.74818642975285,-3.72966710361026,-3.67974873853684,
-3.62148726597934,-3.6008363620686,-3.58706086041255,-3.5731407583426,-3.55167337024444,
-3.52555474014413,-3.45969282291043,-3.42130908118452,-3.40985398308619,
-3.40219898424307,-3.39337584403388,-3.37573324200417,-3.35044936600466,
-3.25350740040407,-3.23342896032252,-3.21988899860481,-3.20587950474091,
-3.18391045542044,-3.15692710154751,-3.08537325705784,-3.05349803705644,
-3.04252959462255,-3.03494038312588,-3.02586770177019,-3.0068014010698,
-2.97841342525751,-2.88489320431958,-2.86566867336246,-2.85226716735696,
-2.83803779896376,-2.814857777735,-2.76064875846864,-2.69018708794146,-2.67757867507596,
-2.67050158217975,-2.66239083688479,-2.64844934808739,-2.6003981139853,
-2.51916721540283,-2.49951326823847,-2.48604394833592,-2.47193328112946,
-2.44940233342474,-2.38777167582929,-2.34349935747219),.UNSPECIFIED.);
#1395=B_SPLINE_CURVE_WITH_KNOTS('',3,(#8486,#8487,#8488,#8489,#8490,#8491,
#8492,#8493,#8494,#8495,#8496,#8497,#8498,#8499,#8500,#8501,#8502,#8503,
#8504,#8505,#8506,#8507,#8508,#8509,#8510,#8511,#8512,#8513,#8514,#8515,
#8516,#8517,#8518,#8519,#8520,#8521,#8522,#8523,#8524,#8525,#8526,#8527,
#8528,#8529,#8530,#8531,#8532,#8533,#8534,#8535,#8536,#8537,#8538,#8539,
#8540,#8541,#8542,#8543,#8544,#8545,#8546,#8547,#8548,#8549,#8550,#8551,
#8552,#8553,#8554,#8555,#8556,#8557,#8558,#8559,#8560,#8561,#8562,#8563,
#8564,#8565,#8566,#8567,#8568,#8569,#8570,#8571,#8572,#8573,#8574,#8575,
#8576,#8577,#8578,#8579,#8580,#8581,#8582,#8583,#8584,#8585,#8586,#8587,
#8588,#8589,#8590,#8591,#8592,#8593,#8594,#8595,#8596,#8597,#8598,#8599,
#8600,#8601,#8602,#8603,#8604,#8605,#8606,#8607,#8608,#8609,#8610,#8611,
#8612,#8613,#8614,#8615,#8616,#8617,#8618,#8619,#8620,#8621,#8622,#8623,
#8624,#8625,#8626,#8627,#8628,#8629,#8630,#8631,#8632,#8633,#8634,#8635,
#8636,#8637,#8638,#8639,#8640,#8641,#8642,#8643,#8644,#8645,#8646,#8647,
#8648,#8649),.UNSPECIFIED.,.F.,.F.,(4,2,2,2,2,2,2,2,2,2,2,2,2,2,2,2,2,2,
2,2,2,2,2,2,2,2,2,2,2,2,2,2,2,2,2,2,2,2,2,2,2,2,2,2,2,2,2,2,2,2,2,2,2,2,
2,2,2,2,2,2,2,2,2,2,2,2,2,2,2,2,2,2,2,2,2,2,2,2,2,2,2,4),(-9.66952787558574,
-9.62868542371412,-9.60520062981699,-9.58844533869582,-9.57980828371517,
-9.57222901153777,-9.56059480413288,-9.5170778567058,-9.43763536439442,
-9.41252443129322,-9.39798885206807,-9.38466240087352,-9.36651121024875,
-9.31294936426819,-9.2386478440979,-9.22184860523329,-9.21320585112177,
-9.20563196293017,-9.19402541406683,-9.15136526291876,-9.07126042488672,
-9.04599378470264,-9.03142938571179,-9.01811100797761,-9.00002543686721,
-8.94863083498729,-8.87500555804877,-8.85628683614255,-8.84729887989887,
-8.83973898748868,-8.82876790080423,-8.79659998462749,-8.72534295999101,
-8.69843461298902,-8.67652777274758,-8.66257503441782,-8.64910702303971,
-8.62917941511827,-8.53970141911645,-8.4958980082845,-8.48434227946981,
-8.4766999086319,-8.46799791967759,-8.45088493681171,-8.3830111739851,-8.32401611422044,
-8.30569223340769,-8.29234017454075,-8.27786956648423,-8.2531273293098,
-8.16209894991134,-8.13861306244888,-8.1218569329555,-8.11322081777102,
-8.10564173854272,-8.0940105026094,-8.05065722445383,-7.97106403955552,
-7.94591453942605,-7.9313693142187,-7.91804111436483,-7.89989863184858,
-7.8467945305261,-7.77463105200812,-7.75614643313473,-7.74719805924447,
-7.73962754296779,-7.72857957716986,-7.69604972364799,-7.62518263866841,
-7.59832788401122,-7.57645115790679,-7.56250267368732,-7.54902878339568,
-7.52907323922341,-7.45052320627916,-7.40075949487996,-7.38665625180731,
-7.37853516625404,-7.37055265491604,-7.35713706650612,-7.32614666109582),
 .UNSPECIFIED.);
#1396=B_SPLINE_CURVE_WITH_KNOTS('',3,(#8654,#8655,#8656,#8657,#8658,#8659,
#8660,#8661,#8662,#8663,#8664,#8665,#8666,#8667,#8668,#8669,#8670,#8671,
#8672,#8673,#8674,#8675,#8676,#8677,#8678,#8679,#8680,#8681,#8682,#8683,
#8684,#8685,#8686,#8687,#8688,#8689,#8690,#8691,#8692,#8693,#8694,#8695,
#8696,#8697,#8698,#8699,#8700,#8701,#8702,#8703,#8704,#8705,#8706,#8707,
#8708,#8709,#8710,#8711,#8712,#8713,#8714,#8715,#8716,#8717,#8718,#8719,
#8720,#8721,#8722,#8723,#8724,#8725,#8726,#8727,#8728,#8729,#8730,#8731,
#8732,#8733,#8734,#8735,#8736,#8737,#8738,#8739,#8740,#8741,#8742,#8743,
#8744,#8745,#8746,#8747,#8748,#8749,#8750,#8751,#8752,#8753,#8754,#8755,
#8756,#8757,#8758,#8759,#8760,#8761,#8762,#8763,#8764,#8765,#8766,#8767,
#8768,#8769,#8770,#8771,#8772,#8773,#8774,#8775,#8776,#8777,#8778,#8779,
#8780,#8781,#8782,#8783,#8784,#8785,#8786,#8787,#8788,#8789,#8790,#8791,
#8792,#8793,#8794,#8795,#8796,#8797,#8798,#8799,#8800,#8801,#8802,#8803,
#8804,#8805,#8806,#8807,#8808,#8809,#8810,#8811,#8812,#8813,#8814,#8815,
#8816,#8817,#8818,#8819),.UNSPECIFIED.,.F.,.F.,(4,2,2,2,2,2,2,2,2,2,2,2,
2,2,2,2,2,2,2,2,2,2,2,2,2,2,2,2,2,2,2,2,2,2,2,2,2,2,2,2,2,2,2,2,2,2,2,2,
2,2,2,2,2,2,2,2,2,2,2,2,2,2,2,2,2,2,2,2,2,2,2,2,2,2,2,2,2,2,2,2,2,2,4),
(-7.03092428991815,-6.97855283092003,-6.9263091663785,-6.90343298259714,
-6.88925830885356,-6.87582481163164,-6.85640239143679,-6.77333102668129,
-6.72630900129152,-6.71248092785882,-6.70439254001495,-6.69630206458313,
-6.68246413762466,-6.63222946623531,-6.57807897662565,-6.554145369954,-6.53397925550643,
-6.52028767087055,-6.50791875477817,-6.48747398280066,-6.43534194700939,
-6.38047727199338,-6.36110356835586,-6.34646347389874,-6.33821192318486,
-6.33026471659157,-6.31714721189776,-6.25137040240187,-6.19216694575456,
-6.16968526743576,-6.1555819194505,-6.14210405022866,-6.12240866899558,
-6.04140145475523,-6.0057936227912,-5.98440903922514,-5.97471869973732,
-5.9672018270527,-5.95727813229174,-5.93262002789266,-5.88946728917574,
-5.82201903183326,-5.80124641436259,-5.78744961801039,-5.7735531340635,
-5.75221782649401,-5.72632447723042,-5.66182519233804,-5.62189284919537,
-5.61029382386929,-5.60269250544359,-5.59396870881027,-5.57687042216555,
-5.55271825777665,-5.50690128728101,-5.45467183960923,-5.43422541324809,
-5.42185618649729,-5.40816452564173,-5.3879993507525,-5.31231040573843,
-5.2598117547567,-5.24583363617778,-5.23771458731285,-5.22965305611284,
-5.21596019245505,-5.17012076798599,-5.08502266380873,-5.06588440242545,
-5.05249442002963,-5.0382359272281,-5.01490587903616,-4.97003309320845,
-4.89123397820596,-4.8782316604893,-4.87030666715579,-4.86202490906503,
-4.8472341505162,-4.82758384494265,-4.77097978873096,-4.71615769979187,
-4.69792986251239,-4.6872551568627),.UNSPECIFIED.);
#1397=B_SPLINE_CURVE_WITH_KNOTS('',3,(#8820,#8821,#8822,#8823,#8824,#8825,
#8826,#8827,#8828,#8829,#8830,#8831,#8832,#8833,#8834,#8835,#8836,#8837,
#8838,#8839,#8840,#8841,#8842,#8843,#8844,#8845,#8846,#8847,#8848,#8849,
#8850,#8851,#8852,#8853,#8854,#8855,#8856,#8857,#8858,#8859,#8860,#8861,
#8862,#8863,#8864,#8865,#8866,#8867,#8868,#8869,#8870,#8871,#8872,#8873,
#8874,#8875,#8876,#8877,#8878,#8879,#8880,#8881,#8882,#8883,#8884,#8885,
#8886,#8887,#8888,#8889,#8890,#8891,#8892,#8893,#8894,#8895,#8896,#8897,
#8898,#8899,#8900,#8901,#8902,#8903,#8904,#8905,#8906,#8907,#8908,#8909,
#8910,#8911,#8912,#8913,#8914,#8915,#8916,#8917,#8918,#8919,#8920,#8921,
#8922,#8923,#8924,#8925,#8926,#8927,#8928,#8929,#8930,#8931,#8932,#8933,
#8934,#8935,#8936,#8937,#8938,#8939,#8940,#8941,#8942,#8943,#8944,#8945,
#8946,#8947,#8948,#8949,#8950,#8951,#8952,#8953,#8954,#8955,#8956,#8957,
#8958,#8959,#8960,#8961,#8962,#8963,#8964,#8965,#8966,#8967,#8968,#8969,
#8970,#8971,#8972,#8973,#8974,#8975,#8976,#8977,#8978,#8979),
 .UNSPECIFIED.,.F.,.F.,(4,2,2,2,2,2,2,2,2,2,2,2,2,2,2,2,2,2,2,2,2,2,2,2,
2,2,2,2,2,2,2,2,2,2,2,2,2,2,2,2,2,2,2,2,2,2,2,2,2,2,2,2,2,2,2,2,2,2,2,2,
2,2,2,2,2,2,2,2,2,2,2,2,2,2,2,2,2,2,2,4),(-7.32614666109582,-7.28096698223301,
-7.23562803637869,-7.21162934426962,-7.19729251320309,-7.18388375068752,
-7.16518217490911,-7.07722444883571,-7.03289792320862,-7.01940820560591,
-7.01141074740473,-7.00330563531193,-6.98928302806448,-6.93614518328078,
-6.8652480833897,-6.84317515560592,-6.82919042136076,-6.81574073928767,
-6.79593493623575,-6.71611341835179,-6.67992048340898,-6.6643005392503,
-6.65179695153731,-6.64399069092723,-6.63563088050373,-6.62032620712114,
-6.55055504570233,-6.49490052330849,-6.47460941120627,-6.46094246774894,
-6.44866670606722,-6.42855563745406,-6.33050714358575,-6.3058821414785,
-6.28856916654671,-6.27982905235152,-6.27219739126771,-6.26072068633731,
-6.22143949391177,-6.15631346069807,-6.13034405198082,-6.10898157803086,
-6.0951242581727,-6.08141294441578,-6.06087434513043,-6.00605848692176,
-5.93686821031972,-5.92097174994566,-5.91249654995843,-5.90475289072757,
-5.8926001789557,-5.83630947403731,-5.76145077257432,-5.74111113201973,
-5.72879829778636,-5.71516775213148,-5.69510030327021,-5.64110693300335,
-5.56611671133825,-5.55249555007277,-5.54447069556817,-5.53639182697379,
-5.52250401970487,-5.4747323679861,-5.39293308176922,-5.37338080834743,
-5.3599708437162,-5.3459196567532,-5.32349191688792,-5.26930329735693,-5.19693781019109,
-5.1845653948362,-5.17754835921317,-5.16942952970917,-5.15534350812577,
-5.10575287413854,-5.02695703768258,-5.00703131203136,-4.99356017536515,
-4.98211504750834),.UNSPECIFIED.);
#1398=B_SPLINE_CURVE_WITH_KNOTS('',3,(#8984,#8985,#8986,#8987,#8988,#8989,
#8990,#8991,#8992,#8993,#8994,#8995,#8996,#8997,#8998,#8999,#9000,#9001,
#9002,#9003,#9004,#9005,#9006,#9007,#9008,#9009,#9010,#9011,#9012,#9013,
#9014,#9015,#9016,#9017,#9018,#9019,#9020,#9021,#9022,#9023,#9024,#9025,
#9026,#9027,#9028,#9029,#9030,#9031,#9032,#9033,#9034,#9035,#9036,#9037,
#9038,#9039,#9040,#9041,#9042,#9043,#9044,#9045,#9046,#9047,#9048,#9049,
#9050,#9051,#9052,#9053,#9054,#9055,#9056,#9057,#9058,#9059,#9060,#9061,
#9062,#9063,#9064,#9065,#9066,#9067,#9068,#9069,#9070,#9071,#9072,#9073,
#9074,#9075,#9076,#9077,#9078,#9079,#9080,#9081,#9082,#9083,#9084,#9085,
#9086,#9087,#9088,#9089,#9090,#9091,#9092,#9093,#9094,#9095,#9096,#9097,
#9098,#9099,#9100,#9101,#9102,#9103,#9104,#9105,#9106,#9107,#9108,#9109,
#9110,#9111,#9112,#9113,#9114,#9115,#9116,#9117,#9118,#9119,#9120,#9121,
#9122,#9123,#9124,#9125,#9126,#9127,#9128,#9129,#9130,#9131,#9132,#9133,
#9134,#9135,#9136,#9137,#9138,#9139,#9140,#9141,#9142,#9143,#9144,#9145,
#9146,#9147),.UNSPECIFIED.,.F.,.F.,(4,2,2,2,2,2,2,2,2,2,2,2,2,2,2,2,2,2,
2,2,2,2,2,2,2,2,2,2,2,2,2,2,2,2,2,2,2,2,2,2,2,2,2,2,2,2,2,2,2,2,2,2,2,2,
2,2,2,2,2,2,2,2,2,2,2,2,2,2,2,2,2,2,2,2,2,2,2,2,2,2,2,4),(-9.37444697003052,
-9.36860397369544,-9.32240173150912,-9.29849118483135,-9.28151276112979,
-9.27281267140479,-9.26520583183669,-9.25356126267184,-9.2107091024805,
-9.13071309151711,-9.10548397620025,-9.09088184965157,-9.07748882582584,
-9.05922923026725,-9.00257070167362,-8.9259559883791,-8.9123957957723,-8.90436198580832,
-8.89621588766257,-8.88210060219873,-8.81098892561669,-8.7547756043323,
-8.73437099593029,-8.72063943506135,-8.70830829152862,-8.68810220976385,
-8.61149871851205,-8.5561222885708,-8.54418314931867,-8.53645223412902,
-8.52783466528434,-8.51130300976799,-8.44279842169963,-8.38776072769088,
-8.36751487256203,-8.35381126284092,-8.34145724310435,-8.32109916431765,
-8.24603712495091,-8.18947470268103,-8.17752065648051,-8.16978766483035,
-8.16117659025836,-8.14467861603178,-8.06941895795403,-8.02739637637241,
-8.00397748130146,-7.98970468931823,-7.97632563747552,-7.95724656237035,
-7.87170706103843,-7.82609223850768,-7.8124264037268,-7.80437132627203,
-7.79624833559249,-7.78224667498632,-7.72949532573729,-7.65826525661566,
-7.6361217363585,-7.62208137192172,-7.60856501126946,-7.58862503459442,
-7.50964021201676,-7.46018559008857,-7.44609043288053,-7.43794855465407,
-7.42991066299454,-7.41633158194777,-7.34105716007606,-7.30218464586766,
-7.27405119537271,-7.25893610676225,-7.24566259847408,-7.22872678051576,
-7.18881191312969,-7.11805910413513,-7.09647688090981,-7.08066848294191,
-7.07218839087097,-7.06448383369831,-7.05225199715093,-7.03092428991815),
 .UNSPECIFIED.);
#1399=B_SPLINE_CURVE_WITH_KNOTS('',3,(#9148,#9149,#9150,#9151,#9152,#9153,
#9154,#9155,#9156,#9157,#9158,#9159,#9160,#9161,#9162,#9163,#9164,#9165,
#9166,#9167,#9168,#9169,#9170,#9171,#9172,#9173,#9174,#9175,#9176,#9177,
#9178,#9179,#9180,#9181,#9182,#9183,#9184,#9185,#9186,#9187,#9188,#9189,
#9190,#9191,#9192,#9193,#9194,#9195,#9196,#9197,#9198,#9199,#9200,#9201,
#9202,#9203,#9204,#9205,#9206,#9207,#9208,#9209,#9210,#9211,#9212,#9213,
#9214,#9215,#9216,#9217,#9218,#9219,#9220,#9221,#9222,#9223,#9224,#9225,
#9226,#9227,#9228,#9229,#9230,#9231,#9232,#9233,#9234,#9235,#9236,#9237,
#9238,#9239,#9240,#9241,#9242,#9243,#9244,#9245,#9246,#9247,#9248,#9249,
#9250,#9251,#9252,#9253,#9254,#9255,#9256,#9257,#9258,#9259,#9260,#9261,
#9262,#9263,#9264,#9265,#9266,#9267,#9268,#9269,#9270,#9271,#9272,#9273,
#9274,#9275,#9276,#9277,#9278,#9279,#9280,#9281,#9282,#9283,#9284,#9285,
#9286,#9287,#9288,#9289,#9290,#9291,#9292,#9293,#9294,#9295,#9296,#9297,
#9298,#9299,#9300,#9301,#9302,#9303,#9304,#9305,#9306,#9307,#9308,#9309,
#9310,#9311,#9312,#9313,#9314,#9315),.UNSPECIFIED.,.F.,.F.,(4,2,2,2,2,2,
2,2,2,2,2,2,2,2,2,2,2,2,2,2,2,2,2,2,2,2,2,2,2,2,2,2,2,2,2,2,2,2,2,2,2,2,
2,2,2,2,2,2,2,2,2,2,2,2,2,2,2,2,2,2,2,2,2,2,2,2,2,2,2,2,2,2,2,2,2,2,2,2,
2,2,2,2,2,4),(-4.98211504750834,-4.97960063193846,-4.95767565633769,-4.93073742230588,
-4.85935336811027,-4.82722732298744,-4.81625866099638,-4.80869677205353,
-4.79970127835455,-4.78095312169327,-4.753247623603,-4.68632185495199,-4.65136073286413,
-4.63500893476475,-4.62184838259256,-4.60624279295363,-4.57488647608268,
-4.52845309893571,-4.46513173709856,-4.45187972741629,-4.44392892090097,
-4.43576821840269,-4.42147248844589,-4.40271013950669,-4.35133310384803,
-4.29487929009314,-4.27431309268189,-4.26059668695628,-4.24674418205149,
-4.22541069965359,-4.19948872683417,-4.13467796516697,-4.09494221816735,
-4.0834447470089,-4.07588466633776,-4.0671875456654,-4.05011034884746,-4.02597442541414,
-3.98013192947666,-3.92785853677376,-3.90744713109667,-3.89512343885818,
-3.88150545087404,-3.86150946815811,-3.80802560135013,-3.73209523135118,
-3.71862757412871,-3.71063378109328,-3.70252226173147,-3.68847150651585,
-3.63920649586705,-3.5598911169119,-3.54002811680221,-3.52656777128116,
-3.51259426797233,-3.49059036191807,-3.46351470430398,-3.3911513437316,
-3.36007613184864,-3.34920897924011,-3.3416594071886,-3.33260637130064,
-3.31352175143696,-3.28506136826114,-3.19168175786884,-3.17245815755866,
-3.15910160745751,-3.14496299393442,-3.12205151671813,-3.07705551532191,
-2.99731067183335,-2.98448858784473,-2.9766218488312,-2.96835271732448,
-2.95351112578539,-2.93374400027773,-2.87627457967711,-2.82246247762319,
-2.80430138815174,-2.79096846613929,-2.77642633681938,-2.75130610660706,
-2.6718338395991,-2.63816549894618),.UNSPECIFIED.);
#1400=B_SPLINE_CURVE_WITH_KNOTS('',3,(#9320,#9321,#9322,#9323,#9324,#9325,
#9326,#9327,#9328,#9329,#9330,#9331,#9332,#9333,#9334,#9335,#9336,#9337,
#9338,#9339,#9340,#9341,#9342,#9343,#9344,#9345,#9346,#9347,#9348,#9349,
#9350,#9351,#9352,#9353,#9354,#9355,#9356,#9357,#9358,#9359,#9360,#9361,
#9362,#9363,#9364,#9365,#9366,#9367,#9368,#9369,#9370,#9371,#9372,#9373,
#9374,#9375,#9376,#9377,#9378,#9379,#9380,#9381,#9382,#9383,#9384,#9385,
#9386,#9387,#9388,#9389,#9390,#9391,#9392,#9393,#9394,#9395,#9396,#9397,
#9398,#9399,#9400,#9401,#9402,#9403,#9404,#9405,#9406,#9407,#9408,#9409,
#9410,#9411,#9412,#9413,#9414,#9415,#9416,#9417,#9418,#9419,#9420,#9421,
#9422,#9423,#9424,#9425,#9426,#9427,#9428,#9429,#9430,#9431,#9432,#9433,
#9434,#9435,#9436,#9437,#9438,#9439,#9440,#9441,#9442,#9443,#9444,#9445,
#9446,#9447,#9448,#9449,#9450,#9451,#9452,#9453,#9454,#9455,#9456,#9457,
#9458,#9459,#9460,#9461,#9462,#9463,#9464,#9465,#9466,#9467,#9468,#9469,
#9470,#9471,#9472,#9473,#9474,#9475,#9476,#9477,#9478,#9479,#9480,#9481,
#9482,#9483),.UNSPECIFIED.,.F.,.F.,(4,2,2,2,2,2,2,2,2,2,2,2,2,2,2,2,2,2,
2,2,2,2,2,2,2,2,2,2,2,2,2,2,2,2,2,2,2,2,2,2,2,2,2,2,2,2,2,2,2,2,2,2,2,2,
2,2,2,2,2,2,2,2,2,2,2,2,2,2,2,2,2,2,2,2,2,2,2,2,2,2,2,4),(-11.7176550926435,
-11.6925733333226,-11.670571262262,-11.6565557431794,-11.6430192663134,
-11.6229712773436,-11.543612482416,-11.4936466144152,-11.4795004301893,
-11.4713674999825,-11.4634062931843,-11.4500711400182,-11.3734355996136,
-11.320362171509,-11.3004333139884,-11.2868375303002,-11.2745205372655,
-11.2540919076865,-11.2014722057254,-11.146861212341,-11.1275458236573,
-11.112950609905,-11.1047354431383,-11.0967929517176,-11.0837127825482,
-11.0054137050487,-10.9602462437258,-10.9369010099404,-10.9226173072797,
-10.9091894597464,-10.8899633117181,-10.7920467278553,-10.7664454448966,
-10.7486491603722,-10.7397812883413,-10.7321194339839,-10.7206742944183,
-10.6824566401323,-10.6165618956935,-10.5904516488257,-10.5689918274307,
-10.5550779902243,-10.5413098404039,-10.5206744784597,-10.4633509001598,
-10.4125741270717,-10.3938986263645,-10.3796419541323,-10.3714719607649,
-10.364441687959,-10.3520919246372,-10.2794662596866,-10.2263183271194,
-10.2034913183482,-10.1893322088993,-10.175904787544,-10.1564765109787,
-10.0735119782026,-10.026436619268,-10.0126063537849,-10.0045206903181,
-9.99742920909095,-9.98473853621118,-9.91504126037811,-9.85921237518751,
-9.836600994619,-9.82247262646748,-9.8090067897254,-9.78939512477712,-9.70780528753865,
-9.65995952470061,-9.64603852627451,-9.63792983587098,-9.62985702579027,
-9.61610426939685,-9.54192921750345,-9.48758843057746,-9.46743861757221,
-9.45375197493255,-9.44138383733526,-9.42093171973615,-9.37444697003052),
 .UNSPECIFIED.);
#1401=B_SPLINE_CURVE_WITH_KNOTS('',3,(#9484,#9485,#9486,#9487,#9488,#9489,
#9490,#9491,#9492,#9493,#9494,#9495,#9496,#9497,#9498,#9499,#9500,#9501,
#9502,#9503,#9504,#9505,#9506,#9507,#9508,#9509,#9510,#9511,#9512,#9513,
#9514,#9515,#9516,#9517,#9518,#9519,#9520,#9521,#9522,#9523,#9524,#9525,
#9526,#9527,#9528,#9529,#9530,#9531,#9532,#9533,#9534,#9535,#9536,#9537,
#9538,#9539,#9540,#9541,#9542,#9543,#9544,#9545,#9546,#9547,#9548,#9549,
#9550,#9551,#9552,#9553,#9554,#9555,#9556,#9557,#9558,#9559,#9560,#9561,
#9562,#9563,#9564,#9565,#9566,#9567,#9568,#9569,#9570,#9571,#9572,#9573,
#9574,#9575,#9576,#9577,#9578,#9579,#9580,#9581,#9582,#9583,#9584,#9585,
#9586,#9587,#9588,#9589,#9590,#9591,#9592,#9593,#9594,#9595,#9596,#9597,
#9598,#9599,#9600,#9601,#9602,#9603,#9604,#9605,#9606,#9607,#9608,#9609,
#9610,#9611,#9612,#9613,#9614,#9615,#9616,#9617,#9618,#9619,#9620,#9621,
#9622,#9623,#9624,#9625,#9626,#9627,#9628,#9629,#9630,#9631,#9632,#9633,
#9634,#9635,#9636,#9637,#9638,#9639,#9640,#9641,#9642,#9643,#9644,#9645,
#9646,#9647,#9648,#9649,#9650,#9651,#9652,#9653,#9654,#9655),
 .UNSPECIFIED.,.F.,.F.,(4,2,2,2,2,2,2,2,2,2,2,2,2,2,2,2,2,2,2,2,2,2,2,2,
2,2,2,2,2,2,2,2,2,2,2,2,2,2,2,2,2,2,2,2,2,2,2,2,2,2,2,2,2,2,2,2,2,2,2,2,
2,2,2,2,2,2,2,2,2,2,2,2,2,2,2,2,2,2,2,2,2,2,2,2,2,4),(-2.63816549894618,
-2.62822464334572,-2.61658219791459,-2.60900017022781,-2.60036573047471,
-2.58362511651739,-2.56017465258522,-2.46956214919072,-2.44456443123561,
-2.43004529991365,-2.41670594128353,-2.39849216605184,-2.3418328786306,
-2.26461197727369,-2.25136149568447,-2.24341146337504,-2.23525097355374,
-2.22095508195867,-2.20219194203138,-2.15080563245531,-2.09437897628173,
-2.07381523531863,-2.06009979804973,-2.04624769011226,-2.02491345165107,
-1.99898954580249,-1.93416028527984,-1.89446338860352,-1.88296602777026,
-1.87540645377818,-1.86671073380068,-1.84963730658322,-1.82550784494192,
-1.77966425287867,-1.72739480904774,-1.70698577409659,-1.69466374500704,
-1.68104782246321,-1.66105548792797,-1.60758673920447,-1.53164143219895,
-1.51817873402861,-1.5101867868185,-1.50207668553401,-1.48802753064419,
-1.43876669091307,-1.35943609955817,-1.33957528102245,-1.3261168029736,
-1.31214570165233,-1.29014682869026,-1.26307812357526,-1.19074732853763,
-1.15965160743421,-1.14878298140033,-1.14123255301325,-1.13217663974462,
-1.11308486336267,-1.08460847547084,-0.991339465378589,-0.972104214822802,
-0.958743359160055,-0.944602771071675,-0.921693086199137,-0.864661332780008,
-0.797171307040493,-0.784244819127981,-0.776357916275508,-0.768121397819388,
-0.753429496506319,-0.733937027354846,-0.678193138830802,-0.622238280397907,
-0.604040641736677,-0.590709636511149,-0.576197034069192,-0.551206792878598,
-0.518680002167478,-0.470510111833088,-0.42789133709684,-0.416286394664346,
-0.408715000213329,-0.4000793088898,-0.383307782692103,-0.35979250168467,
-0.294449080646368),.UNSPECIFIED.);
#1402=B_SPLINE_CURVE_WITH_KNOTS('',3,(#9658,#9659,#9660,#9661,#9662,#9663,
#9664,#9665,#9666,#9667,#9668,#9669,#9670,#9671,#9672,#9673,#9674,#9675,
#9676,#9677,#9678,#9679,#9680,#9681,#9682,#9683),.UNSPECIFIED.,.F.,.F.,
(4,2,2,2,2,2,2,2,2,2,2,2,4),(-0.294449080646368,-0.268387930386075,-0.243820374475458,
-0.22938269985925,-0.216021618487623,-0.19762188835446,-0.136808234456886,
-0.063856534004244,-0.0508349045132531,-0.0429260567403737,-0.0359882159395519,
-0.0276063209548247,-0.000158070576422473),.UNSPECIFIED.);
#1403=B_SPLINE_CURVE_WITH_KNOTS('',3,(#9685,#9686,#9687,#9688,#9689,#9690,
#9691,#9692,#9693,#9694,#9695,#9696,#9697,#9698,#9699,#9700,#9701,#9702,
#9703,#9704,#9705,#9706,#9707,#9708,#9709,#9710,#9711,#9712,#9713,#9714,
#9715,#9716,#9717,#9718,#9719,#9720,#9721,#9722,#9723,#9724,#9725,#9726,
#9727,#9728,#9729,#9730,#9731,#9732,#9733,#9734,#9735,#9736,#9737,#9738,
#9739,#9740,#9741,#9742,#9743,#9744,#9745,#9746,#9747,#9748,#9749,#9750,
#9751,#9752,#9753,#9754,#9755,#9756,#9757,#9758,#9759,#9760,#9761,#9762,
#9763,#9764,#9765,#9766,#9767,#9768,#9769,#9770,#9771,#9772,#9773,#9774,
#9775,#9776,#9777,#9778,#9779,#9780,#9781,#9782,#9783,#9784,#9785,#9786,
#9787,#9788,#9789,#9790,#9791,#9792,#9793,#9794,#9795,#9796,#9797,#9798,
#9799,#9800,#9801,#9802,#9803,#9804,#9805,#9806,#9807,#9808,#9809,#9810,
#9811,#9812,#9813,#9814,#9815,#9816,#9817,#9818,#9819,#9820,#9821,#9822,
#9823,#9824,#9825,#9826,#9827,#9828,#9829,#9830,#9831,#9832,#9833,#9834,
#9835,#9836,#9837,#9838,#9839,#9840,#9841,#9842,#9843,#9844,#9845,#9846,
#9847,#9848,#9849,#9850,#9851,#9852,#9853,#9854,#9855,#9856,#9857,#9858,
#9859,#9860,#9861,#9862,#9863,#9864,#9865,#9866,#9867,#9868,#9869,#9870,
#9871),.UNSPECIFIED.,.F.,.F.,(4,3,3,3,3,3,3,3,3,3,3,3,3,3,3,3,3,3,3,3,3,
3,3,3,3,3,3,3,3,3,3,3,3,3,3,3,3,3,3,3,3,3,3,3,3,3,3,3,3,3,3,3,3,3,3,3,3,
3,3,3,3,3,4),(47.12389017617,47.212634310815,47.3012804954036,47.3898536706167,
47.4783881657889,47.5669071783758,47.6554338879542,47.7440444285322,47.8326984185048,
47.9214901286793,47.9900165621361,47.9900533884742,48.0705655363816,48.079878475582,
48.1696262134622,48.2592844383872,48.3488804771275,48.4384437308739,48.5279963661167,
48.6175605357571,48.707215576596,48.7969155021056,48.8867636103351,48.9684752652717,
48.9731232496585,48.9731599923317,49.0537238943936,49.0631813344679,49.1531246430108,
49.2429775986181,49.3327663197129,49.4225209467818,49.5122634308969,49.6020157083635,
49.6918549669428,49.7817372622351,49.8717626820065,49.956229937181,49.9562646843143,
50.0372658835791,50.0464205997571,50.1364989391249,50.2264891614412,50.3164179156243,
50.4063141963529,50.4961997669363,50.5860963769902,50.6760809951302,50.766109414171,
50.8562806870504,50.9393366247034,50.9393761753254,51.0185464949487,51.0273822113533,
51.1153142003882,51.2043285952813,51.2921153635596,51.379874703757,51.4676302816496,
51.5575800511205,51.6454454055357,51.7364373825343,51.8184455727287),
 .UNSPECIFIED.);
#1404=B_SPLINE_CURVE_WITH_KNOTS('',3,(#9875,#9876,#9877,#9878,#9879,#9880,
#9881,#9882,#9883,#9884,#9885,#9886,#9887,#9888,#9889,#9890,#9891,#9892,
#9893,#9894,#9895,#9896,#9897,#9898,#9899,#9900,#9901,#9902,#9903,#9904,
#9905,#9906,#9907,#9908,#9909,#9910,#9911,#9912,#9913,#9914,#9915,#9916,
#9917,#9918,#9919,#9920,#9921,#9922,#9923,#9924,#9925,#9926,#9927,#9928,
#9929,#9930,#9931,#9932,#9933,#9934,#9935,#9936,#9937,#9938,#9939,#9940,
#9941,#9942,#9943,#9944,#9945,#9946,#9947,#9948,#9949,#9950,#9951,#9952,
#9953,#9954,#9955,#9956,#9957,#9958,#9959,#9960,#9961,#9962,#9963,#9964,
#9965,#9966,#9967,#9968,#9969,#9970,#9971,#9972,#9973,#9974,#9975,#9976,
#9977,#9978,#9979,#9980,#9981,#9982,#9983,#9984,#9985,#9986,#9987,#9988,
#9989,#9990,#9991,#9992,#9993,#9994,#9995,#9996,#9997,#9998,#9999,#10000,
#10001,#10002,#10003,#10004,#10005,#10006,#10007,#10008,#10009,#10010,#10011,
#10012,#10013,#10014,#10015,#10016),.UNSPECIFIED.,.F.,.F.,(4,3,3,3,3,3,
3,3,3,3,3,3,3,3,3,3,3,3,3,3,3,3,3,3,3,3,3,3,3,3,3,3,3,3,3,3,3,3,3,3,3,3,
3,3,3,3,3,4),(47.1238898038469,47.2174754673338,47.3111680100548,47.4050579725487,
47.4990543518043,47.5843560963284,47.5932435711771,47.6391053165797,47.639145354705,
47.7202593538192,47.7282111079036,47.8171624892304,47.9060250358962,47.9955534116876,
48.0843273344302,48.1730941115943,48.2618766705276,48.3519705134526,48.4409057141138,
48.5315788781706,48.6115449556694,48.6222159452476,48.6222520422274,48.704134821478,
48.7134731108222,48.8045685913688,48.8955611216527,48.9864649966019,49.0773190413066,
49.1681435703031,49.2589588697564,49.3498243415436,49.4407136971665,49.5317037438762,
49.6053370119153,49.6053587297499,49.69634898757,49.7872668551369,49.8781345589675,
49.9689726175072,50.0598150491269,50.0969120735111,50.0969186132547,50.1985524169299,
50.3004232260078,50.4023379611143,50.5041923151378,50.5884654172723),
 .UNSPECIFIED.);
#1405=B_SPLINE_CURVE_WITH_KNOTS('',3,(#10017,#10018,#10019,#10020,#10021,
#10022,#10023,#10024,#10025,#10026,#10027,#10028,#10029,#10030,#10031,#10032,
#10033,#10034,#10035,#10036,#10037,#10038,#10039,#10040),.UNSPECIFIED.,
 .F.,.F.,(4,2,2,2,2,2,2,2,2,2,2,4),(-12.0120719037212,-12.0010573616161,
-11.9867119540422,-11.904250798684,-11.8715813211036,-11.850683020791,-11.8411538380416,
-11.8334529515479,-11.822560800604,-11.7920652487739,-11.7196340744173,
-11.7176550926435),.UNSPECIFIED.);
#1406=B_SPLINE_CURVE_WITH_KNOTS('',3,(#10044,#10045,#10046,#10047,#10048,
#10049,#10050,#10051,#10052,#10053,#10054,#10055,#10056,#10057,#10058,#10059,
#10060,#10061,#10062,#10063,#10064,#10065,#10066,#10067,#10068,#10069,#10070,
#10071,#10072,#10073,#10074,#10075,#10076,#10077,#10078,#10079,#10080,#10081,
#10082,#10083,#10084,#10085,#10086,#10087,#10088,#10089,#10090,#10091,#10092,
#10093,#10094,#10095,#10096,#10097,#10098,#10099,#10100,#10101,#10102,#10103,
#10104,#10105,#10106,#10107,#10108,#10109,#10110,#10111,#10112,#10113,#10114,
#10115,#10116,#10117,#10118,#10119,#10120,#10121,#10122,#10123,#10124,#10125,
#10126,#10127,#10128,#10129,#10130,#10131,#10132,#10133,#10134,#10135,#10136,
#10137,#10138,#10139,#10140,#10141,#10142,#10143,#10144,#10145,#10146,#10147,
#10148,#10149,#10150,#10151,#10152,#10153,#10154,#10155,#10156,#10157,#10158,
#10159,#10160,#10161),.UNSPECIFIED.,.F.,.F.,(4,3,3,3,3,3,3,3,3,3,3,3,3,
3,3,3,3,3,3,3,3,3,3,3,3,3,3,3,3,3,3,3,3,3,3,3,3,3,3,4),(-4.09289414414334,
-4.00843569444614,-3.95955978524779,-3.9324557935787,-3.93242675008978,
-3.85384525365456,-3.84608852572687,-3.75985370563718,-3.67370105299863,
-3.60241376041841,-3.58315342919472,-3.51290061676997,-3.49709435009809,
-3.41104793156076,-3.33194995829287,-3.32499509288074,-3.25893240679908,
-3.2389167535879,-3.15274805448362,-3.06652690774132,-2.98763571046433,
-2.98018641192965,-2.94935374406167,-2.94932006256734,-2.87252712645479,
-2.86503523867605,-2.7808550431761,-2.69675631414078,-2.63498082505163,
-2.61271378948831,-2.54090460291134,-2.52869995275755,-2.41037007810133,
-2.36067529736391,-2.29985971128565,-2.27657679923735,-2.20652088686618,
-2.1924341240595,-2.10817127163918,-2.0620931210805),.UNSPECIFIED.);
#1407=B_SPLINE_CURVE_WITH_KNOTS('',3,(#10165,#10166,#10167,#10168,#10169,
#10170,#10171,#10172,#10173,#10174,#10175,#10176,#10177,#10178,#10179,#10180,
#10181,#10182,#10183,#10184,#10185,#10186,#10187,#10188,#10189,#10190),
 .UNSPECIFIED.,.F.,.F.,(4,2,2,2,2,2,2,2,2,2,2,2,4),(0.,0.0194959022105328,
0.0584392371124239,0.114822265828151,0.164960797084267,0.246283622826695,
0.323295648367368,0.397518421465989,0.41363588735925,0.425864804055925,
0.436832758233511,0.455647012980926,0.492598869825882),.UNSPECIFIED.);
#1408=B_SPLINE_CURVE_WITH_KNOTS('',3,(#10192,#10193,#10194,#10195,#10196,
#10197,#10198,#10199,#10200,#10201,#10202,#10203,#10204,#10205,#10206,#10207,
#10208,#10209,#10210,#10211,#10212,#10213,#10214,#10215,#10216,#10217,#10218,
#10219,#10220,#10221,#10222,#10223,#10224,#10225,#10226,#10227,#10228,#10229,
#10230,#10231,#10232,#10233,#10234,#10235,#10236,#10237,#10238,#10239,#10240,
#10241,#10242,#10243,#10244,#10245,#10246,#10247,#10248,#10249,#10250,#10251,
#10252,#10253,#10254,#10255,#10256,#10257,#10258,#10259,#10260,#10261,#10262,
#10263,#10264,#10265,#10266,#10267,#10268,#10269,#10270,#10271,#10272,#10273,
#10274,#10275,#10276,#10277,#10278,#10279,#10280,#10281,#10282,#10283,#10284,
#10285,#10286,#10287,#10288,#10289,#10290,#10291,#10292,#10293,#10294,#10295,
#10296,#10297,#10298,#10299,#10300,#10301,#10302,#10303,#10304,#10305,#10306,
#10307,#10308,#10309,#10310,#10311,#10312,#10313,#10314,#10315,#10316,#10317,
#10318,#10319,#10320,#10321,#10322,#10323,#10324,#10325,#10326,#10327,#10328,
#10329,#10330,#10331,#10332,#10333,#10334,#10335,#10336,#10337,#10338,#10339,
#10340,#10341,#10342,#10343,#10344,#10345,#10346,#10347,#10348,#10349,#10350,
#10351,#10352,#10353,#10354,#10355,#10356,#10357,#10358,#10359,#10360,#10361,
#10362,#10363,#10364,#10365,#10366,#10367,#10368,#10369,#10370,#10371,#10372,
#10373,#10374,#10375,#10376,#10377,#10378,#10379,#10380,#10381,#10382,#10383,
#10384,#10385,#10386,#10387,#10388,#10389,#10390,#10391,#10392,#10393,#10394,
#10395,#10396,#10397,#10398,#10399,#10400,#10401,#10402,#10403,#10404,#10405,
#10406,#10407,#10408,#10409,#10410,#10411,#10412,#10413,#10414,#10415,#10416,
#10417,#10418,#10419,#10420,#10421,#10422,#10423,#10424,#10425,#10426,#10427,
#10428,#10429,#10430,#10431,#10432,#10433,#10434,#10435,#10436,#10437,#10438,
#10439,#10440,#10441,#10442,#10443,#10444,#10445,#10446,#10447,#10448,#10449,
#10450,#10451,#10452,#10453,#10454,#10455,#10456,#10457,#10458,#10459,#10460,
#10461,#10462,#10463,#10464,#10465,#10466,#10467,#10468,#10469,#10470,#10471,
#10472,#10473,#10474,#10475,#10476,#10477,#10478,#10479,#10480,#10481,#10482,
#10483,#10484,#10485,#10486,#10487,#10488,#10489,#10490,#10491,#10492,#10493,
#10494,#10495,#10496,#10497,#10498,#10499,#10500,#10501,#10502,#10503,#10504,
#10505,#10506,#10507,#10508,#10509,#10510,#10511,#10512,#10513,#10514,#10515,
#10516,#10517,#10518,#10519),.UNSPECIFIED.,.F.,.F.,(4,3,3,3,3,3,3,3,3,3,
3,3,3,3,3,3,3,3,3,3,3,3,3,3,3,3,3,3,3,3,3,3,3,3,3,3,3,3,3,3,3,3,3,3,3,3,
3,3,3,3,3,3,3,3,3,3,3,3,3,3,3,3,3,3,3,3,3,3,3,3,3,3,3,3,3,3,3,3,3,3,3,3,
3,3,3,3,3,3,3,3,3,3,3,3,3,3,3,3,3,3,3,3,3,3,3,3,3,3,3,4),(1.10990013830804,
1.1961286058751,1.25196222134668,1.28229535123711,1.39349992939904,1.51275424662582,
1.54068094018495,1.62683182926768,1.68212521043177,1.71308212960078,1.79938293490773,
1.88094723079734,1.88582928212476,1.96618291867898,1.96621337504489,2.04375333511063,
2.05153108173538,2.13673294970428,2.22184143229054,2.28102853375086,2.30687888662215,
2.3918736400768,2.50546630057955,2.56182185653531,2.61816392998536,2.64681554817045,
2.73189761684025,2.81702879702236,2.89630232944247,2.90228614623796,2.94928686442096,
2.94932006256734,3.0274018791421,3.03565805991247,3.12189270046458,3.2080452208331,
3.29077173342695,3.29859291199018,3.36018397709367,3.38465197828492,3.47069842778444,
3.55675134115351,3.61893904656727,3.64282979885581,3.72899868109771,3.81522004855201,
3.89464542126761,3.90156081956687,3.93239753466603,3.93242675008978,4.01081868217623,
4.01862531663163,4.10472062379942,4.19073408969261,4.25235268719438,4.27668705919604,
4.36260993804403,4.4766480016078,4.53443659800429,4.60851037805321,4.62037886781216,
4.70641359734286,4.79250118256877,4.87185479163746,4.87871238538384,4.91550255891886,
4.91553343761223,4.99363650524933,5.00156375899611,5.08748769640701,5.17332689219006,
5.23826602356694,5.25910291179368,5.33123427756829,5.3448454961129,5.45886531939574,
5.51630566495775,5.59065164197529,5.60206211830088,5.68790953458488,5.77380869437548,
5.85324777795459,5.85983139642645,5.8986091808827,5.89864012513467,5.97682534817979,
5.98479447136155,6.07084407042382,6.15681040430506,6.22339442557936,6.24271488026911,
6.31278432489712,6.32858741328564,6.442683640289,6.50031001604005,6.58619867867155,
6.67217852283113,6.75821041676436,6.83768892414904,6.84436517205843,6.88171630337422,
6.88174681265712,6.96162680560509,6.97139414465698,7.06090018627908,7.15023013756892,
7.21226088232711,7.23945576258717,7.32855559990409,7.39308541414175),
 .UNSPECIFIED.);
#1409=B_SPLINE_CURVE_WITH_KNOTS('',3,(#10521,#10522,#10523,#10524,#10525,
#10526,#10527,#10528,#10529,#10530,#10531,#10532,#10533,#10534,#10535,#10536,
#10537,#10538,#10539,#10540,#10541,#10542,#10543,#10544,#10545,#10546,#10547,
#10548,#10549,#10550,#10551,#10552,#10553,#10554,#10555,#10556,#10557,#10558,
#10559,#10560,#10561,#10562,#10563,#10564,#10565,#10566,#10567,#10568,#10569,
#10570,#10571,#10572,#10573,#10574,#10575,#10576,#10577,#10578,#10579,#10580,
#10581,#10582,#10583,#10584,#10585,#10586,#10587,#10588,#10589,#10590,#10591,
#10592,#10593,#10594,#10595,#10596,#10597,#10598,#10599,#10600,#10601,#10602,
#10603,#10604,#10605,#10606,#10607,#10608,#10609,#10610,#10611,#10612,#10613,
#10614,#10615,#10616,#10617,#10618,#10619,#10620,#10621,#10622,#10623,#10624,
#10625,#10626,#10627,#10628,#10629,#10630,#10631,#10632,#10633,#10634,#10635,
#10636,#10637,#10638,#10639,#10640,#10641,#10642,#10643,#10644,#10645,#10646,
#10647,#10648,#10649,#10650,#10651,#10652,#10653,#10654,#10655,#10656,#10657,
#10658,#10659,#10660,#10661,#10662,#10663,#10664,#10665,#10666,#10667,#10668,
#10669,#10670,#10671,#10672,#10673,#10674,#10675,#10676,#10677,#10678,#10679,
#10680,#10681,#10682,#10683,#10684,#10685,#10686,#10687,#10688,#10689,#10690,
#10691,#10692,#10693,#10694,#10695,#10696,#10697,#10698,#10699,#10700,#10701,
#10702,#10703,#10704,#10705,#10706,#10707,#10708,#10709,#10710,#10711,#10712,
#10713,#10714,#10715,#10716,#10717,#10718,#10719,#10720,#10721,#10722,#10723,
#10724,#10725,#10726,#10727,#10728,#10729,#10730,#10731,#10732,#10733,#10734,
#10735,#10736,#10737,#10738,#10739,#10740,#10741,#10742,#10743,#10744,#10745,
#10746,#10747,#10748,#10749,#10750,#10751,#10752,#10753,#10754,#10755,#10756,
#10757,#10758,#10759,#10760,#10761,#10762,#10763,#10764,#10765,#10766,#10767,
#10768,#10769,#10770,#10771,#10772,#10773,#10774,#10775,#10776,#10777,#10778,
#10779,#10780,#10781,#10782,#10783,#10784,#10785,#10786,#10787,#10788,#10789,
#10790,#10791,#10792,#10793,#10794,#10795,#10796,#10797,#10798,#10799,#10800,
#10801,#10802,#10803,#10804,#10805,#10806,#10807,#10808,#10809,#10810,#10811,
#10812,#10813,#10814,#10815,#10816,#10817,#10818,#10819,#10820,#10821,#10822,
#10823,#10824,#10825,#10826,#10827,#10828,#10829,#10830,#10831,#10832,#10833,
#10834,#10835,#10836,#10837,#10838,#10839,#10840,#10841,#10842,#10843,#10844,
#10845,#10846,#10847,#10848,#10849,#10850,#10851,#10852,#10853,#10854,#10855,
#10856,#10857,#10858,#10859,#10860),.UNSPECIFIED.,.F.,.F.,(4,3,3,3,3,3,
3,3,3,3,3,3,3,3,3,3,3,3,3,3,3,3,3,3,3,3,3,3,3,3,3,3,3,3,3,3,3,3,3,3,3,3,
3,3,3,3,3,3,3,3,3,3,3,3,3,3,3,3,3,3,3,3,3,3,3,3,3,3,3,3,3,3,3,3,3,3,3,3,
3,3,3,3,3,3,3,3,3,3,3,3,3,3,3,3,3,3,3,3,3,3,3,3,3,3,3,3,3,3,3,3,3,3,3,4),
(7.3930854143344,7.46038550079444,7.48366125998094,7.5789593200306,7.66991850903281,
7.75593207956134,7.7610068757006,7.84118324163327,7.85228887176144,7.86482277028161,
7.86485350017956,7.94303010247594,7.95096567356472,8.0369726336412,8.12289591723387,
8.18821517045417,8.20875698581783,8.28063321315669,8.29458574146171,8.40864764903128,
8.4662201866803,8.54699140015504,8.55206456429625,8.63800018005379,8.7239878182005,
8.80343769099625,8.81009865991351,8.84792947320008,8.84796018770201,8.92614885835429,
8.93408705165396,9.02010890939336,9.10604727849447,9.17147498951346,9.19192360144347,
9.26368552584356,9.27776780665372,9.39183773100395,9.44943348524598,9.53529361359441,
9.62124502178279,9.70724849768268,9.78670119867335,9.79337510940081,9.83103620527342,
9.83106687522445,9.90925690090911,9.91718938261793,10.0032068469648,10.0891407914262,
10.1543660154415,10.1750126640201,10.2471131548751,10.2608523972262,10.3749177581416,
10.4325091004347,10.5137737355322,10.5183647351718,10.604311670713,10.6903106799034,
10.7697586512753,10.7764328728798,10.8141428649052,10.8141735627469,10.892359956357,
10.9002949112415,10.9863111869436,11.0722439146069,11.1375528108811,11.1581145438086,
11.2300578046464,11.2439529984951,11.3580189170255,11.4156070814413,11.4970857186119,
11.5014613770805,11.5874069521317,11.6734045867373,11.752854448271,11.7595253953439,
11.7972495568869,11.7972802502693,11.8754682914925,11.8834032732732,11.9694212484686,
12.0553556984052,12.120667522524,12.1412280704876,12.2131749688845,12.2270682923214,
12.3411350037324,12.3987259514211,12.4845820522888,12.5705294391601,12.6565288918185,
12.7359788613518,12.7426515122888,12.7803562486784,12.7803869377918,12.8579454211869,
12.8655355434748,12.9505796553732,13.0355418164815,13.1021756909872,13.1204452668709,
13.1890182990663,13.20531838703,13.3238563297698,13.3750546099121,13.4395618577246,
13.4600018316116,13.5449901073353,13.6300921524228,13.6762707211195),
 .UNSPECIFIED.);
#1410=B_SPLINE_CURVE_WITH_KNOTS('',3,(#10862,#10863,#10864,#10865,#10866,
#10867,#10868,#10869,#10870,#10871,#10872,#10873,#10874,#10875,#10876,#10877,
#10878,#10879,#10880,#10881,#10882,#10883,#10884,#10885,#10886,#10887,#10888,
#10889,#10890,#10891,#10892,#10893,#10894,#10895,#10896,#10897,#10898,#10899,
#10900,#10901,#10902,#10903,#10904,#10905,#10906,#10907,#10908,#10909,#10910,
#10911,#10912,#10913,#10914,#10915,#10916,#10917,#10918,#10919,#10920,#10921,
#10922,#10923,#10924,#10925,#10926,#10927,#10928,#10929,#10930,#10931,#10932,
#10933,#10934,#10935,#10936,#10937,#10938,#10939,#10940,#10941,#10942,#10943,
#10944,#10945,#10946,#10947,#10948,#10949,#10950,#10951,#10952,#10953,#10954,
#10955,#10956,#10957,#10958,#10959,#10960,#10961,#10962,#10963,#10964,#10965,
#10966,#10967,#10968,#10969,#10970,#10971,#10972,#10973,#10974,#10975,#10976,
#10977,#10978,#10979,#10980,#10981,#10982,#10983,#10984,#10985,#10986,#10987,
#10988,#10989,#10990,#10991,#10992,#10993,#10994,#10995,#10996,#10997,#10998,
#10999,#11000,#11001,#11002,#11003,#11004,#11005,#11006,#11007,#11008,#11009,
#11010,#11011,#11012,#11013,#11014,#11015,#11016,#11017,#11018,#11019,#11020,
#11021,#11022,#11023,#11024,#11025,#11026,#11027,#11028,#11029,#11030,#11031,
#11032,#11033,#11034,#11035,#11036,#11037,#11038,#11039,#11040,#11041,#11042,
#11043,#11044,#11045,#11046,#11047,#11048,#11049,#11050,#11051,#11052,#11053,
#11054,#11055,#11056,#11057,#11058,#11059,#11060,#11061,#11062,#11063,#11064,
#11065,#11066,#11067,#11068,#11069,#11070,#11071,#11072,#11073,#11074,#11075,
#11076,#11077,#11078,#11079,#11080,#11081,#11082,#11083,#11084,#11085,#11086,
#11087,#11088,#11089,#11090,#11091,#11092,#11093,#11094,#11095,#11096,#11097,
#11098,#11099,#11100,#11101,#11102,#11103,#11104,#11105,#11106,#11107,#11108,
#11109,#11110,#11111,#11112,#11113,#11114,#11115,#11116,#11117,#11118,#11119,
#11120,#11121,#11122,#11123,#11124,#11125,#11126,#11127,#11128,#11129,#11130,
#11131,#11132,#11133,#11134,#11135,#11136,#11137,#11138,#11139,#11140,#11141,
#11142,#11143,#11144,#11145,#11146,#11147,#11148,#11149,#11150,#11151,#11152,
#11153,#11154,#11155,#11156,#11157,#11158,#11159,#11160,#11161,#11162,#11163,
#11164,#11165,#11166,#11167,#11168,#11169,#11170,#11171,#11172,#11173,#11174,
#11175,#11176,#11177,#11178,#11179,#11180,#11181,#11182,#11183,#11184,#11185,
#11186,#11187,#11188,#11189,#11190,#11191,#11192,#11193,#11194,#11195,#11196,
#11197,#11198,#11199,#11200,#11201,#11202,#11203,#11204,#11205,#11206,#11207),
 .UNSPECIFIED.,.F.,.F.,(4,3,3,3,3,3,3,3,3,3,3,3,3,3,3,3,3,3,3,3,3,3,3,3,
3,3,3,3,3,3,3,3,3,3,3,3,3,3,3,3,3,3,3,3,3,3,3,3,3,3,3,3,3,3,3,3,3,3,3,3,
3,3,3,3,3,3,3,3,3,3,3,3,3,3,3,3,3,3,3,3,3,3,3,3,3,3,3,3,3,3,3,3,3,3,3,3,
3,3,3,3,3,3,3,3,3,3,3,3,3,3,3,3,3,3,3,4),(13.6762707213213,13.7634629327955,
13.7634936253142,13.8416812604774,13.8496159580763,13.9356332340953,14.0215669768221,
14.0868681734509,14.1074386345513,14.179400911131,14.1932781340374,14.3073443975024,
14.3649343349407,14.4464660882827,14.4507897015138,14.536736353218,14.6227350692125,
14.7021847788391,14.7088569571122,14.7465696211511,14.7466003128367,14.8247881614203,
14.8327228290312,14.9187402913841,15.0046742231037,15.069974604919,15.0905460722461,
15.1625107839159,15.1763857660457,15.2904521017495,15.3480423606136,15.4295863405157,
15.4338979261233,15.5198447777085,15.6058436943958,15.6852933898944,15.6919657824959,
15.7296763090431,15.7297070003591,15.8078948248047,15.8158294310186,15.9018468068606,
15.9877806512044,16.0530788150397,16.0736524122154,16.1456206491793,16.1594920170861,
16.2735582856674,16.3311484324836,16.4126770413684,16.4170039079444,16.5029506695495,
16.5889494961742,16.6683991387936,16.675071494867,16.7127829961687,16.7128136878816,
16.7910014741668,16.7989361209402,16.8849534990149,16.9708873454232,17.0361869085138,
17.0567591083282,17.1287248468944,17.1425987148302,17.2566650025967,17.3142551329948,
17.3957891316664,17.4001106095863,17.4860573720587,17.5720561994008,17.6515058741772,
17.6581781985741,17.6958896838184,17.695920375404,17.7741081883125,17.7820428278235,
17.8680602255835,17.953994091976,18.0192934276472,18.0398658751388,18.1118321246165,
18.1257055022317,18.2397717958319,18.2973619621599,18.3788967293656,18.3832174598805,
18.4691642436063,18.555163092302,18.6346127623353,18.6412851127977,18.6789963713672,
18.6790270629265,18.7572148705848,18.7651495041418,18.8511668905623,18.9371007454944,
19.002399871327,19.0229725170903,19.0949390859491,19.1088121325003,19.2228784179173,
19.2804685688698,19.3620017052309,19.3663240547399,19.4522708266136,19.5382696634402,
19.6177193281047,19.6243916721438,19.6621030588424,19.6621337504489,19.7455613159664,
19.7659686645438,19.8527584971793,19.8686725452676,19.9594558713002),
 .UNSPECIFIED.);
#1411=B_SPLINE_CURVE_WITH_KNOTS('',3,(#11209,#11210,#11211,#11212,#11213,
#11214,#11215,#11216,#11217,#11218,#11219,#11220,#11221,#11222,#11223,#11224,
#11225,#11226,#11227,#11228,#11229,#11230,#11231,#11232,#11233,#11234,#11235,
#11236,#11237,#11238,#11239,#11240,#11241,#11242,#11243,#11244,#11245,#11246,
#11247,#11248,#11249,#11250,#11251,#11252,#11253,#11254,#11255,#11256,#11257,
#11258,#11259,#11260,#11261,#11262,#11263,#11264,#11265,#11266,#11267,#11268,
#11269,#11270,#11271,#11272,#11273,#11274,#11275,#11276,#11277,#11278,#11279,
#11280,#11281,#11282,#11283,#11284,#11285,#11286,#11287,#11288,#11289,#11290,
#11291,#11292,#11293,#11294,#11295,#11296,#11297,#11298,#11299,#11300,#11301,
#11302,#11303,#11304,#11305,#11306,#11307,#11308,#11309,#11310,#11311,#11312,
#11313,#11314,#11315,#11316,#11317,#11318,#11319,#11320,#11321,#11322,#11323,
#11324,#11325,#11326,#11327,#11328,#11329,#11330,#11331,#11332,#11333,#11334,
#11335,#11336,#11337,#11338,#11339,#11340,#11341,#11342,#11343,#11344,#11345,
#11346,#11347,#11348,#11349,#11350,#11351,#11352,#11353,#11354,#11355,#11356,
#11357,#11358,#11359,#11360,#11361,#11362,#11363,#11364,#11365,#11366,#11367,
#11368,#11369,#11370,#11371,#11372,#11373,#11374,#11375,#11376,#11377,#11378,
#11379,#11380,#11381,#11382,#11383,#11384,#11385,#11386,#11387,#11388,#11389,
#11390,#11391,#11392,#11393,#11394,#11395,#11396,#11397,#11398,#11399,#11400,
#11401,#11402,#11403,#11404,#11405,#11406,#11407,#11408,#11409,#11410,#11411,
#11412,#11413,#11414,#11415,#11416,#11417,#11418,#11419,#11420,#11421,#11422,
#11423,#11424,#11425,#11426,#11427,#11428,#11429,#11430,#11431,#11432,#11433,
#11434,#11435,#11436,#11437),.UNSPECIFIED.,.F.,.F.,(4,3,3,3,3,3,3,3,3,3,
3,3,3,3,3,3,3,3,3,3,3,3,3,3,3,3,3,3,3,3,3,3,3,3,3,3,3,3,3,3,3,3,3,3,3,3,
3,3,3,3,3,3,3,3,3,3,3,3,3,3,3,3,3,3,3,3,3,3,3,3,3,3,3,3,3,3,4),(19.9594560285009,
20.0451790796847,20.1305458428908,20.2159059621089,20.3012792146047,20.3872695204463,
20.4727722942822,20.5590063661267,20.6452404379713,20.7313628836198,20.8173802745045,
20.903314133926,20.9891859100309,21.0750255299629,21.1608511074417,21.246681975391,
21.3325374657882,21.4184842421596,21.5044830834734,21.5906050966088,21.6283471254938,
21.7144695676753,21.8004869550807,21.8864208110143,21.9722925836273,22.0581322000745,
22.1439577740739,22.2297886385524,22.3156441254915,22.4015908984418,22.4875897363515,
22.5737117461376,22.6114538130162,22.6975762542529,22.783593640691,22.8695274956365,
22.9553992672416,23.0412388826549,23.1270644556048,23.2128953190199,23.2987508048819,
23.3846975767421,23.4706964135524,23.5568184222344,23.5945605005387,23.6806829535161,
23.7667003517293,23.8526342184696,23.9385060018757,24.0243456290561,24.110171213748,
24.196002088868,24.2818575863844,24.3678043697609,24.453803218024,24.5399252379628,
24.5776671880611,24.6637896198065,24.7498069968154,24.8357408424047,24.9216126047368,
25.007452211033,25.0932777749654,25.1791086294714,25.2649641065426,25.350910869837,
25.436909698198,25.5230316986823,25.5607738755836,25.6464658524267,25.7320583612643,
25.8175712968715,25.9030244902211,25.9884489916975,26.0738534974488,26.1592909000781,
26.2426413356805),.UNSPECIFIED.);
#1412=B_SPLINE_CURVE_WITH_KNOTS('',3,(#11439,#11440,#11441,#11442,#11443,
#11444,#11445,#11446,#11447,#11448,#11449,#11450,#11451,#11452,#11453,#11454,
#11455,#11456,#11457,#11458,#11459,#11460,#11461,#11462,#11463,#11464,#11465,
#11466,#11467,#11468,#11469,#11470,#11471,#11472,#11473,#11474,#11475,#11476,
#11477,#11478,#11479,#11480,#11481,#11482,#11483,#11484,#11485,#11486,#11487,
#11488,#11489,#11490,#11491,#11492,#11493,#11494,#11495,#11496,#11497,#11498,
#11499,#11500,#11501,#11502,#11503,#11504,#11505,#11506,#11507,#11508,#11509,
#11510,#11511,#11512,#11513,#11514,#11515,#11516,#11517,#11518,#11519,#11520,
#11521,#11522,#11523,#11524,#11525,#11526,#11527,#11528,#11529,#11530,#11531,
#11532,#11533,#11534,#11535,#11536,#11537,#11538,#11539,#11540,#11541,#11542,
#11543,#11544,#11545,#11546,#11547,#11548,#11549,#11550,#11551,#11552,#11553,
#11554,#11555,#11556,#11557,#11558,#11559,#11560,#11561,#11562,#11563,#11564,
#11565,#11566,#11567,#11568,#11569,#11570,#11571,#11572,#11573,#11574,#11575,
#11576,#11577,#11578,#11579,#11580,#11581,#11582,#11583,#11584,#11585,#11586,
#11587,#11588,#11589,#11590,#11591,#11592,#11593,#11594,#11595,#11596,#11597,
#11598,#11599,#11600,#11601,#11602,#11603,#11604,#11605,#11606,#11607,#11608,
#11609,#11610,#11611,#11612,#11613,#11614,#11615,#11616,#11617,#11618,#11619,
#11620,#11621,#11622,#11623,#11624,#11625,#11626,#11627,#11628,#11629,#11630,
#11631,#11632,#11633,#11634,#11635,#11636,#11637,#11638,#11639,#11640,#11641,
#11642,#11643,#11644,#11645,#11646,#11647,#11648,#11649,#11650,#11651,#11652,
#11653,#11654,#11655,#11656,#11657,#11658,#11659,#11660,#11661,#11662,#11663,
#11664,#11665,#11666,#11667,#11668,#11669,#11670,#11671,#11672,#11673,#11674,
#11675,#11676,#11677,#11678,#11679,#11680,#11681,#11682,#11683,#11684,#11685,
#11686,#11687,#11688,#11689,#11690,#11691,#11692,#11693,#11694,#11695,#11696,
#11697,#11698,#11699,#11700,#11701,#11702,#11703,#11704,#11705,#11706,#11707,
#11708,#11709,#11710,#11711,#11712,#11713,#11714,#11715,#11716,#11717,#11718,
#11719,#11720,#11721,#11722,#11723,#11724,#11725,#11726,#11727,#11728,#11729,
#11730,#11731,#11732,#11733,#11734,#11735,#11736,#11737,#11738,#11739,#11740,
#11741,#11742,#11743,#11744,#11745,#11746,#11747,#11748,#11749,#11750,#11751,
#11752,#11753,#11754,#11755,#11756,#11757,#11758,#11759,#11760,#11761,#11762,
#11763,#11764,#11765,#11766,#11767,#11768,#11769,#11770,#11771,#11772,#11773,
#11774,#11775,#11776,#11777,#11778,#11779,#11780,#11781),.UNSPECIFIED.,
 .F.,.F.,(4,3,3,3,3,3,3,3,3,3,3,3,3,3,3,3,3,3,3,3,3,3,3,3,3,3,3,3,3,3,3,
3,3,3,3,3,3,3,3,3,3,3,3,3,3,3,3,3,3,3,3,3,3,3,3,3,3,3,3,3,3,3,3,3,3,3,3,
3,3,3,3,3,3,3,3,3,3,3,3,3,3,3,3,3,3,3,3,3,3,3,3,3,3,3,3,3,3,3,3,3,3,3,3,
3,3,3,3,3,3,3,3,3,3,3,4),(26.242641499509,26.3324415864858,26.3446941768379,
26.4313149906762,26.4478838155214,26.5302507572133,26.5438498718212,26.543880563106,
26.622068448048,26.6300030833935,26.7160205490677,26.8019544833399,26.8672543793336,
26.8878263342683,26.9597921828112,26.9736660287096,27.0877323185049,27.1453226224228,
27.2268738403406,27.2311781864362,27.3171250354588,27.4031239489703,27.4825736061514,
27.4892460329838,27.5269565589012,27.5269872506285,27.6051750106045,27.6131095715702,
27.6991268379978,27.7850605733534,27.8503602927242,27.8709322259246,27.942897926408,
27.9567717235579,28.0708378791915,28.1284279269293,28.2099819216018,28.2142832978237,
28.3002299569284,28.3862286820944,28.4656782525,28.4723505817956,28.5100632455641,
28.5100939381509,28.5882815216702,28.5962163393846,28.6822336845469,28.7681674970097,
28.8334629716548,28.8540392249894,28.9260092202108,28.9398787952556,29.0539453790681,
29.111535138587,29.1929504221305,29.1973905766713,29.2833372997852,29.3693360872299,
29.4487860194801,29.4554580460383,29.4931699369254,29.4932006256733,29.5713891295633,
29.5793236759997,29.6653416733656,29.7512761403407,29.81658196337,29.8371485243456,
29.9091094146335,29.9229887504622,30.0370549240626,30.0946464038566,30.1805024947355,
30.2664498645006,30.3524492959591,30.4318987707329,30.4385718891503,30.4762766193398,
30.4763073131958,30.5544944690055,30.5624285594366,30.6484447521662,30.7343774160621,
30.7996775079718,30.8202480006432,30.8922116034977,30.9060864392999,31.0201517567277,
31.0777405435947,31.1635948766145,31.2495405156828,31.3355382296261,31.4149872318963,
31.4216591403216,31.4593833024249,31.4594140007182,31.5376003722513,31.5455366257588,
31.6315541855686,31.7174882033962,31.7827581688761,31.8033601273273,31.8753555708931,
31.8891998789751,32.0032688426819,32.0608565576179,32.1414714565194,32.1467121493448,
32.2326590112296,32.3186579291363,32.3981099080769,32.4047800046536,32.4424900212834,
32.4425206882407,32.5258266428601),.UNSPECIFIED.);
#1413=B_SPLINE_CURVE_WITH_KNOTS('',3,(#11783,#11784,#11785,#11786,#11787,
#11788,#11789,#11790,#11791,#11792,#11793,#11794,#11795,#11796,#11797,#11798,
#11799,#11800,#11801,#11802,#11803,#11804,#11805,#11806,#11807,#11808,#11809,
#11810,#11811,#11812,#11813,#11814,#11815,#11816,#11817,#11818,#11819,#11820,
#11821,#11822,#11823,#11824,#11825,#11826,#11827,#11828,#11829,#11830,#11831,
#11832,#11833,#11834,#11835,#11836,#11837,#11838,#11839,#11840,#11841,#11842,
#11843,#11844,#11845,#11846,#11847,#11848,#11849,#11850,#11851,#11852,#11853,
#11854,#11855,#11856,#11857,#11858,#11859,#11860,#11861,#11862,#11863,#11864,
#11865,#11866,#11867,#11868,#11869,#11870,#11871,#11872,#11873,#11874,#11875,
#11876,#11877,#11878,#11879,#11880,#11881,#11882,#11883,#11884,#11885,#11886,
#11887,#11888,#11889,#11890,#11891,#11892,#11893,#11894,#11895,#11896,#11897,
#11898,#11899,#11900,#11901,#11902,#11903,#11904,#11905,#11906,#11907,#11908,
#11909,#11910,#11911,#11912,#11913,#11914,#11915,#11916,#11917,#11918,#11919,
#11920,#11921,#11922,#11923,#11924,#11925,#11926,#11927,#11928,#11929,#11930,
#11931,#11932,#11933,#11934,#11935,#11936,#11937,#11938,#11939,#11940,#11941,
#11942,#11943,#11944,#11945,#11946,#11947,#11948,#11949,#11950,#11951,#11952,
#11953,#11954,#11955,#11956,#11957,#11958,#11959,#11960,#11961,#11962,#11963,
#11964,#11965,#11966,#11967,#11968,#11969,#11970,#11971,#11972,#11973,#11974,
#11975,#11976,#11977,#11978,#11979,#11980,#11981,#11982,#11983,#11984,#11985,
#11986,#11987,#11988,#11989,#11990,#11991,#11992,#11993,#11994,#11995,#11996,
#11997,#11998,#11999,#12000,#12001,#12002,#12003,#12004,#12005,#12006,#12007,
#12008,#12009,#12010,#12011,#12012,#12013,#12014,#12015,#12016,#12017,#12018,
#12019,#12020,#12021,#12022,#12023,#12024,#12025,#12026,#12027,#12028,#12029,
#12030,#12031,#12032,#12033,#12034,#12035,#12036,#12037,#12038,#12039,#12040,
#12041,#12042,#12043,#12044,#12045,#12046,#12047,#12048,#12049,#12050,#12051,
#12052,#12053,#12054,#12055,#12056,#12057,#12058,#12059,#12060,#12061,#12062,
#12063,#12064,#12065,#12066,#12067,#12068,#12069,#12070,#12071,#12072,#12073,
#12074,#12075,#12076,#12077,#12078,#12079,#12080,#12081,#12082,#12083,#12084,
#12085,#12086,#12087,#12088,#12089,#12090,#12091,#12092,#12093,#12094,#12095,
#12096,#12097,#12098,#12099,#12100,#12101,#12102,#12103,#12104,#12105,#12106,
#12107,#12108,#12109,#12110,#12111,#12112,#12113,#12114,#12115,#12116,#12117,
#12118,#12119,#12120,#12121,#12122,#12123,#12124,#12125),.UNSPECIFIED.,
 .F.,.F.,(4,3,3,3,3,3,3,3,3,3,3,3,3,3,3,3,3,3,3,3,3,3,3,3,3,3,3,3,3,3,3,
3,3,3,3,3,3,3,3,3,3,3,3,3,3,3,3,3,3,3,3,3,3,3,3,3,3,3,3,3,3,3,3,3,3,3,3,
3,3,3,3,3,3,3,3,3,3,3,3,3,3,3,3,3,3,3,3,3,3,3,3,3,3,3,3,3,3,3,3,3,3,3,3,
3,3,3,3,3,3,3,3,3,3,3,4),(32.5258266430594,32.6109724346887,32.6960210961378,
32.7626267165768,32.7809951098591,32.8492755535054,32.8659214354213,32.9837841938069,
33.0357235442058,33.0955474570151,33.1206397523944,33.2056408545587,33.2906886895505,
33.3702936267599,33.3758609577714,33.4255966563581,33.4256273757631,33.5038076716489,
33.5117386977598,33.5977449669701,33.6836677195876,33.7489468907353,33.7695284165969,
33.8414965542859,33.8553570387069,33.9694167254514,34.0269916614943,34.1083538408373,
34.1128363502318,34.1987724988946,34.2847607974944,34.3642063976649,34.3708724891257,
34.4087033319985,34.4087340632856,34.4869140335835,34.4948626039088,34.5808860086697,
34.6668257949821,34.731910342736,34.7527034050599,34.8248937007329,34.8385487008752,
34.9526382498946,35.0102161927437,35.0858142890628,35.0960770425472,35.1820289830922,
35.2680328840028,35.3475020183578,35.3541597537952,35.3918102649572,35.391840750808,
35.470077668493,35.4779957931001,35.564045956927,35.6500127247878,35.7158985485698,
35.7359175043445,35.807382148658,35.8217901462905,35.9358306049138,35.9935126031944,
36.0794010110302,36.1653804190781,36.2514117725677,36.330834342922,36.3375658326432,
36.3749164460689,36.3749474383305,36.4530570251503,36.4609709985879,36.5468894484378,
36.6327244251594,36.6976322862784,36.7184974902785,36.7906951843131,36.8042390095103,
36.9182650828356,36.9757005755,37.0503973116492,37.0614594912268,37.1473111312689,
37.2332155266954,37.3126454208301,37.3192449713843,37.3580232566258,37.3580541258529,
37.4362146806441,37.4442653932351,37.5303710041113,37.616392385932,37.6802782697322,
37.7023508908437,37.7760215559506,37.7882757520974,37.9025348642431,37.9600997363509,
38.0195474650972,38.0460373477549,38.132064110626,38.2181418243531,38.2977501570041,
38.3043403342073,38.3411317666744,38.3411608133753,38.4219344625309,38.4323669275132,
38.5186731840825,38.5265281831132,38.6173539858577,38.6828524694273,38.7080464538249,
38.7985713335135,38.8090119499132),.UNSPECIFIED.);
#1414=B_SPLINE_CURVE_WITH_KNOTS('',3,(#12127,#12128,#12129,#12130,#12131,
#12132,#12133,#12134,#12135,#12136,#12137,#12138,#12139,#12140,#12141,#12142,
#12143,#12144,#12145,#12146,#12147,#12148,#12149,#12150,#12151,#12152,#12153,
#12154,#12155,#12156,#12157,#12158,#12159,#12160,#12161,#12162,#12163,#12164,
#12165,#12166,#12167,#12168,#12169,#12170,#12171,#12172,#12173,#12174,#12175,
#12176,#12177,#12178,#12179,#12180,#12181,#12182,#12183,#12184,#12185,#12186,
#12187,#12188,#12189,#12190,#12191,#12192,#12193,#12194,#12195,#12196,#12197,
#12198,#12199,#12200,#12201,#12202,#12203,#12204,#12205),.UNSPECIFIED.,
 .F.,.F.,(4,3,3,3,3,3,3,3,3,3,3,3,3,3,3,3,3,3,3,3,3,3,3,3,3,3,4),(38.8090119500397,
38.8859986035339,38.8986001599551,38.9583027320439,38.9882861023177,39.0781574059986,
39.1681251672574,39.2510575887847,39.2582803096457,39.3242338171694,39.3242675008978,
39.4010604352791,39.4085522045926,39.4927322947236,39.5768309331739,39.6386139026977,
39.6608734290088,39.7326664346078,39.7448872573002,39.8632170642639,39.9129119571121,
39.973722445964,39.9970107280833,40.0670781135363,40.0811536853461,40.1654173637519,
40.2123859659494),.UNSPECIFIED.);
#1415=B_SPLINE_CURVE_WITH_KNOTS('',3,(#12209,#12210,#12211,#12212,#12213,
#12214,#12215,#12216,#12217,#12218,#12219,#12220),.UNSPECIFIED.,.F.,.F.,
(4,2,2,2,2,4),(0.,0.0190431087261921,0.0547437896044447,0.10678546066118,
0.157808217256731,0.213640188390348),.UNSPECIFIED.);
#1416=B_SPLINE_CURVE_WITH_KNOTS('',3,(#12222,#12223,#12224,#12225,#12226,
#12227,#12228,#12229,#12230,#12231,#12232,#12233,#12234,#12235,#12236,#12237,
#12238,#12239,#12240,#12241,#12242,#12243,#12244,#12245,#12246,#12247,#12248,
#12249,#12250,#12251,#12252,#12253,#12254,#12255,#12256,#12257,#12258,#12259,
#12260,#12261,#12262,#12263,#12264,#12265,#12266,#12267,#12268,#12269,#12270,
#12271,#12272,#12273,#12274,#12275,#12276,#12277,#12278,#12279,#12280,#12281,
#12282,#12283,#12284,#12285,#12286,#12287,#12288,#12289,#12290,#12291,#12292,
#12293,#12294,#12295,#12296,#12297,#12298,#12299,#12300,#12301,#12302,#12303,
#12304,#12305,#12306,#12307,#12308,#12309,#12310,#12311,#12312,#12313,#12314,
#12315,#12316,#12317,#12318,#12319,#12320,#12321,#12322,#12323,#12324,#12325,
#12326,#12327,#12328,#12329,#12330,#12331,#12332,#12333,#12334,#12335,#12336,
#12337,#12338,#12339,#12340,#12341,#12342,#12343,#12344,#12345,#12346,#12347,
#12348,#12349,#12350,#12351,#12352,#12353,#12354,#12355,#12356,#12357,#12358,
#12359,#12360,#12361,#12362,#12363,#12364,#12365,#12366,#12367,#12368,#12369,
#12370,#12371,#12372,#12373,#12374,#12375,#12376,#12377,#12378,#12379,#12380,
#12381,#12382,#12383,#12384,#12385,#12386,#12387,#12388,#12389,#12390,#12391,
#12392,#12393,#12394,#12395,#12396,#12397,#12398,#12399,#12400,#12401,#12402,
#12403,#12404,#12405,#12406,#12407,#12408,#12409,#12410,#12411,#12412,#12413,
#12414,#12415,#12416,#12417,#12418,#12419,#12420,#12421,#12422,#12423,#12424,
#12425,#12426,#12427,#12428,#12429,#12430,#12431,#12432,#12433,#12434,#12435,
#12436,#12437,#12438,#12439,#12440,#12441,#12442,#12443,#12444,#12445,#12446,
#12447,#12448,#12449,#12450,#12451,#12452,#12453,#12454,#12455,#12456,#12457,
#12458,#12459,#12460,#12461,#12462,#12463,#12464,#12465,#12466,#12467,#12468,
#12469,#12470,#12471,#12472,#12473,#12474,#12475,#12476,#12477,#12478,#12479,
#12480,#12481,#12482,#12483,#12484,#12485,#12486,#12487,#12488,#12489,#12490,
#12491,#12492,#12493,#12494,#12495,#12496,#12497,#12498,#12499,#12500,#12501,
#12502,#12503,#12504,#12505,#12506,#12507,#12508,#12509,#12510,#12511,#12512,
#12513,#12514,#12515,#12516,#12517,#12518,#12519,#12520,#12521,#12522,#12523,
#12524,#12525,#12526,#12527,#12528,#12529,#12530,#12531,#12532,#12533,#12534,
#12535,#12536,#12537,#12538,#12539,#12540,#12541,#12542,#12543,#12544,#12545,
#12546,#12547,#12548,#12549,#12550,#12551,#12552),.UNSPECIFIED.,.F.,.F.,
(4,3,3,3,3,3,3,3,3,3,3,3,3,3,3,3,3,3,3,3,3,3,3,3,3,3,3,3,3,3,3,3,3,3,3,
3,3,3,3,3,3,3,3,3,3,3,3,3,3,3,3,3,3,3,3,3,3,3,3,3,3,3,3,3,3,3,3,3,3,3,3,
3,3,3,3,3,3,3,3,3,3,3,3,3,3,3,3,3,3,3,3,3,3,3,3,3,3,3,3,3,3,3,3,3,3,3,3,
3,3,3,4),(-41.79200593275,-41.7820342197039,-41.7820289155157,-41.6950743300943,
-41.6081223321859,-41.5211282447415,-41.4341127720792,-41.3470146427639,
-41.2905004994869,-41.2904808759427,-41.2098667853675,-41.20336832383,-41.1163307621064,
-41.0585781090169,-41.0293484847566,-40.9391016977146,-40.82443344383,-40.7126439695405,
-40.6782149646209,-40.6237387775751,-40.5911902746634,-40.5040544223173,
-40.4168531658136,-40.3384683697826,-40.329521224308,-40.3074046461754,
-40.3073741884203,-40.2298340840655,-40.2220564467519,-40.1368545416153,
-40.0517460197423,-39.9925639013076,-39.9667085240719,-39.8817137263903,
-39.7681210243195,-39.7117654161815,-39.6554187743151,-39.6267716751265,
-39.5416895547738,-39.4565583215444,-39.3772848419879,-39.3713009176492,
-39.3243006969237,-39.3242675008978,-39.2461857144567,-39.2379295253732,
-39.1516949070862,-39.0655424093964,-38.9828521641219,-38.9749947098938,
-38.9133947084934,-38.8889356671652,-38.8028892415144,-38.7168363522496,
-38.6546592803102,-38.6307579188814,-38.5445890611926,-38.4583677184446,
-38.3789423236917,-38.3720269721772,-38.3411900255245,-38.3411608133754,
-38.2627688277661,-38.2549622066264,-38.1688668587652,-38.0828533517434,
-38.0212440044143,-37.9969003407262,-37.9109774199415,-37.7969393456923,
-37.7391506754001,-37.6651611227124,-37.6532083630363,-37.567173590932,
-37.4810859630649,-37.4017323695988,-37.3948747178714,-37.3580850021048,
-37.3580541258529,-37.279951088596,-37.2720238464053,-37.1860999512967,
-37.1002607981332,-37.0353332851499,-37.0144848214179,-36.9423340886966,
-36.9287422802383,-36.8147224638751,-36.7572821980678,-36.683026967767,
-36.6715257881743,-36.5856784152043,-36.4997792987108,-36.4203402253949,
-36.4137566395602,-36.3749783802581,-36.3749474383305,-36.2974958690074,
-36.2899292270807,-36.2050152151128,-36.1179908982539,-36.0505591832992,
-36.0332183657195,-35.9653932816982,-35.9484752386565,-35.8291557711193,
-35.7750110506216,-35.6901947599964,-35.6053351568716,-35.5203766098291,
-35.5088206802422),.UNSPECIFIED.);
#1417=B_SPLINE_CURVE_WITH_KNOTS('',3,(#12554,#12555,#12556,#12557,#12558,
#12559,#12560,#12561,#12562,#12563,#12564,#12565,#12566,#12567,#12568,#12569,
#12570,#12571,#12572,#12573,#12574,#12575,#12576,#12577,#12578,#12579,#12580,
#12581,#12582,#12583,#12584,#12585,#12586,#12587,#12588,#12589,#12590,#12591,
#12592,#12593,#12594,#12595,#12596,#12597,#12598,#12599,#12600,#12601,#12602,
#12603,#12604,#12605,#12606,#12607,#12608,#12609,#12610,#12611,#12612,#12613,
#12614,#12615,#12616,#12617,#12618,#12619,#12620,#12621,#12622,#12623,#12624,
#12625,#12626,#12627,#12628,#12629,#12630,#12631,#12632,#12633,#12634,#12635,
#12636,#12637,#12638,#12639,#12640,#12641,#12642,#12643,#12644,#12645,#12646,
#12647,#12648,#12649,#12650,#12651,#12652,#12653,#12654,#12655,#12656,#12657,
#12658,#12659,#12660,#12661,#12662,#12663,#12664,#12665,#12666,#12667,#12668,
#12669,#12670,#12671,#12672,#12673,#12674,#12675,#12676,#12677,#12678,#12679,
#12680,#12681,#12682,#12683,#12684,#12685,#12686,#12687,#12688,#12689,#12690,
#12691,#12692,#12693,#12694,#12695,#12696,#12697,#12698,#12699,#12700,#12701,
#12702,#12703,#12704,#12705,#12706,#12707,#12708,#12709,#12710,#12711,#12712,
#12713,#12714,#12715,#12716,#12717,#12718,#12719,#12720,#12721,#12722,#12723,
#12724,#12725,#12726,#12727,#12728,#12729,#12730,#12731,#12732,#12733,#12734,
#12735,#12736,#12737,#12738,#12739,#12740,#12741,#12742,#12743,#12744,#12745,
#12746,#12747,#12748,#12749,#12750,#12751,#12752,#12753,#12754,#12755,#12756,
#12757,#12758,#12759,#12760,#12761,#12762,#12763,#12764,#12765,#12766,#12767,
#12768,#12769,#12770,#12771,#12772,#12773,#12774,#12775,#12776,#12777,#12778,
#12779,#12780,#12781,#12782,#12783,#12784,#12785,#12786,#12787,#12788,#12789,
#12790,#12791,#12792,#12793,#12794,#12795,#12796,#12797,#12798,#12799,#12800,
#12801,#12802,#12803,#12804,#12805,#12806,#12807,#12808,#12809,#12810,#12811,
#12812,#12813,#12814,#12815,#12816,#12817,#12818,#12819,#12820,#12821,#12822,
#12823,#12824,#12825,#12826,#12827,#12828,#12829,#12830,#12831,#12832,#12833,
#12834,#12835,#12836,#12837,#12838,#12839,#12840,#12841,#12842,#12843,#12844,
#12845,#12846,#12847,#12848,#12849,#12850,#12851,#12852,#12853,#12854,#12855,
#12856,#12857,#12858,#12859,#12860,#12861,#12862,#12863,#12864,#12865,#12866,
#12867,#12868,#12869,#12870,#12871,#12872,#12873,#12874,#12875,#12876,#12877,
#12878,#12879,#12880,#12881,#12882,#12883,#12884,#12885,#12886,#12887,#12888,
#12889,#12890,#12891,#12892,#12893,#12894,#12895,#12896,#12897,#12898,#12899),
 .UNSPECIFIED.,.F.,.F.,(4,3,3,3,3,3,3,3,3,3,3,3,3,3,3,3,3,3,3,3,3,3,3,3,
3,3,3,3,3,3,3,3,3,3,3,3,3,3,3,3,3,3,3,3,3,3,3,3,3,3,3,3,3,3,3,3,3,3,3,3,
3,3,3,3,3,3,3,3,3,3,3,3,3,3,3,3,3,3,3,3,3,3,3,3,3,3,3,3,3,3,3,3,3,3,3,3,
3,3,3,3,3,3,3,3,3,3,3,3,3,3,3,3,3,3,3,4),(-35.5088206800413,-35.4252279654651,
-35.3918712573551,-35.391840750808,-35.3136311441657,-35.3057134673612,
-35.2196910812655,-35.1337520760534,-35.0690300403527,-35.0478750102457,
-34.974784245045,-34.9620299050909,-34.8479689727154,-34.7903621339832,
-34.7106196849279,-34.7045008142665,-34.6185480744502,-34.5325431848047,
-34.45310662989,-34.4464150450444,-34.4087647906727,-34.4087340632856,-34.330557471788,
-34.322621901095,-34.2366149523578,-34.1506916802349,-34.0853841922607,
-34.0648306232373,-33.9929355963962,-33.9790018793112,-33.8649399597694,
-33.8073674577515,-33.7267315923107,-33.7215230920524,-33.6355874882297,
-33.5495998620446,-33.4701499889646,-33.4634890322309,-33.4256580877462,
-33.4256273757631,-33.3474387042409,-33.3395005067057,-33.2534786438155,
-33.1675402695245,-33.1021242827212,-33.0816639413529,-33.0098835327419,
-32.9958197308907,-32.8817497850192,-32.8241540417499,-32.7382939081162,
-32.6523424946626,-32.5663390135018,-32.4868863076403,-32.480212396575,
-32.4425513556011,-32.4425206882407,-32.3643306588553,-32.3563981804201,
-32.2703807156258,-32.1844467706973,-32.119233340652,-32.0985748976172,
-32.02645504593,-32.0127351638982,-31.898669787616,-31.8410784596148,-31.7599527945309,
-31.7552228243167,-31.6692758881938,-31.5832768784092,-31.5038289086898,
-31.4971546848244,-31.4594446960179,-31.4594140007183,-31.3812276090757,
-31.3732926541172,-31.2872763803364,-31.20134365462,-31.136046512765,-31.1154730273881,
-31.0435108360474,-31.0296345746987,-30.9155686400612,-30.8579804957934,
-30.7766425020302,-30.7721262021939,-30.6861806291898,-30.6001829966384,
-30.5207331340705,-30.514062190079,-30.4763380040283,-30.4763073131958,
-30.3981192712659,-30.3901842891515,-30.3041663129045,-30.2182318619066,
-30.1529317867028,-30.1323594887544,-30.0603936548166,-30.046519265842,
-29.9324525368224,-29.8748616045711,-29.7933742647299,-29.7890055026128,
-29.7030581146527,-29.6170586609049,-29.5376086899911,-29.5309360393539,
-29.4932313122272,-29.4932006256734,-29.4094094906891,-29.3853784705262,
-29.2988803407037,-29.2791332454367,-29.2256353730422),.UNSPECIFIED.);
#1418=B_SPLINE_CURVE_WITH_KNOTS('',3,(#12901,#12902,#12903,#12904,#12905,
#12906,#12907,#12908,#12909,#12910,#12911,#12912,#12913,#12914,#12915,#12916,
#12917,#12918,#12919,#12920,#12921,#12922,#12923,#12924,#12925,#12926,#12927,
#12928,#12929,#12930,#12931,#12932,#12933,#12934,#12935,#12936,#12937,#12938,
#12939,#12940,#12941,#12942,#12943,#12944,#12945,#12946,#12947,#12948,#12949,
#12950,#12951,#12952,#12953,#12954,#12955,#12956,#12957,#12958,#12959,#12960,
#12961,#12962,#12963,#12964,#12965,#12966,#12967,#12968,#12969,#12970,#12971,
#12972,#12973,#12974,#12975,#12976,#12977,#12978,#12979,#12980,#12981,#12982,
#12983,#12984,#12985,#12986,#12987,#12988,#12989,#12990,#12991,#12992,#12993,
#12994,#12995,#12996,#12997,#12998,#12999,#13000,#13001,#13002,#13003,#13004,
#13005,#13006,#13007,#13008,#13009,#13010,#13011,#13012,#13013,#13014,#13015,
#13016,#13017,#13018,#13019,#13020,#13021,#13022,#13023,#13024,#13025,#13026,
#13027,#13028,#13029,#13030,#13031,#13032,#13033,#13034,#13035,#13036,#13037,
#13038,#13039,#13040,#13041,#13042,#13043,#13044,#13045,#13046,#13047,#13048,
#13049,#13050,#13051,#13052,#13053,#13054,#13055,#13056,#13057,#13058,#13059,
#13060,#13061,#13062,#13063,#13064,#13065,#13066,#13067,#13068,#13069,#13070,
#13071,#13072,#13073,#13074,#13075,#13076,#13077,#13078,#13079,#13080,#13081,
#13082,#13083,#13084,#13085,#13086,#13087,#13088,#13089,#13090,#13091,#13092,
#13093,#13094,#13095,#13096,#13097,#13098,#13099,#13100,#13101,#13102,#13103,
#13104,#13105,#13106,#13107,#13108,#13109,#13110,#13111,#13112,#13113,#13114,
#13115,#13116,#13117,#13118,#13119,#13120,#13121,#13122,#13123,#13124,#13125,
#13126,#13127,#13128,#13129,#13130,#13131,#13132,#13133,#13134,#13135,#13136,
#13137,#13138,#13139,#13140,#13141,#13142,#13143,#13144,#13145,#13146,#13147,
#13148,#13149,#13150,#13151,#13152,#13153,#13154,#13155,#13156,#13157,#13158,
#13159,#13160,#13161,#13162,#13163,#13164,#13165,#13166,#13167,#13168,#13169,
#13170,#13171,#13172,#13173,#13174,#13175,#13176,#13177,#13178,#13179,#13180,
#13181,#13182,#13183,#13184,#13185,#13186,#13187,#13188,#13189,#13190,#13191,
#13192,#13193,#13194,#13195,#13196,#13197,#13198,#13199,#13200,#13201,#13202,
#13203,#13204,#13205,#13206,#13207,#13208,#13209,#13210,#13211,#13212,#13213,
#13214,#13215,#13216,#13217,#13218,#13219,#13220,#13221,#13222,#13223,#13224,
#13225,#13226,#13227,#13228,#13229,#13230,#13231,#13232,#13233,#13234,#13235,
#13236,#13237,#13238,#13239,#13240,#13241,#13242,#13243),.UNSPECIFIED.,
 .F.,.F.,(4,3,3,3,3,3,3,3,3,3,3,3,3,3,3,3,3,3,3,3,3,3,3,3,3,3,3,3,3,3,3,
3,3,3,3,3,3,3,3,3,3,3,3,3,3,3,3,3,3,3,3,3,3,3,3,3,3,3,3,3,3,3,3,3,3,3,3,
3,3,3,3,3,3,3,3,3,3,3,3,3,3,3,3,3,3,3,3,3,3,3,3,3,3,3,3,3,3,3,3,3,3,3,3,
3,3,3,3,3,3,3,3,3,3,3,4),(-29.2256353728617,-29.1630398051076,-29.1361926935229,
-29.0511260979808,-28.9353197102132,-28.88102302201,-28.8096224637669,-28.7959463909764,
-28.7107799985853,-28.6255612560834,-28.5471267143894,-28.5402214425233,
-28.5101246280994,-28.5100939381509,-28.4319063030582,-28.4239716056522,
-28.3379543299007,-28.2520205874456,-28.1867311485525,-28.1661489299919,
-28.0941676710746,-28.0803094307853,-27.9662431504983,-27.9086532304487,
-27.8272624804431,-27.822797864162,-27.7368512127461,-27.6508524970411,
-27.5714027865234,-27.5647306094304,-27.5270179397605,-27.5269872506285,
-27.4487994016289,-27.4408647342574,-27.3548472717257,-27.2689133398253,
-27.2036247164402,-27.1830414905009,-27.1110577884387,-27.0972017965172,
-26.9831354437756,-26.9255452015783,-26.8441422998106,-26.8396896358817,
-26.7537427841098,-26.6677438672355,-26.5882941708569,-26.5816217789496,
-26.5439112518674,-26.543880563106,-26.4656927382692,-26.4577581324764,
-26.3717407566645,-26.2858069123508,-26.2205205104771,-26.1999351513698,
-26.1279479104358,-26.1140955465289,-26.0000292610949,-25.9424391311903,
-25.8610515026847,-25.856583655759,-25.7706368941827,-25.6846380675869,
-25.6051884242157,-25.598516068922,-25.5608045647431,-25.5607738755836,
-25.4825860890327,-25.4746514425571,-25.3886340645148,-25.3027002181393,
-25.2374124146042,-25.216828455268,-25.1448437226632,-25.1309888488002,
-25.0169225441039,-24.9593324307051,-24.8779394469641,-24.8734769541487,
-24.7875301917118,-24.7015313644052,-24.6220816888261,-24.6154093652677,
-24.5776978770929,-24.5776671880611,-24.4994793748203,-24.4915447356144,
-24.4055273378264,-24.3195934714057,-24.2543058956866,-24.2337216882146,
-24.1617364426304,-24.1478820610932,-24.033815750705,-23.9762256011071,
-23.8948318526411,-23.8903701033575,-23.8044233196025,-23.7184244708774,
-23.6389748000345,-23.6323024503526,-23.594591189544,-23.5945605005387,
-23.5164327751492,-23.5084383448351,-23.4224191446739,-23.3364834599017,
-23.2711382794071,-23.2506119149563,-23.1786842672096,-23.1647805520879,
-23.0511684817596,-22.9931527448939,-22.9424500656821),.UNSPECIFIED.);
#1419=B_SPLINE_CURVE_WITH_KNOTS('',3,(#13245,#13246,#13247,#13248,#13249,
#13250,#13251,#13252,#13253,#13254,#13255,#13256,#13257,#13258,#13259,#13260,
#13261,#13262,#13263,#13264,#13265,#13266,#13267,#13268,#13269,#13270,#13271,
#13272,#13273,#13274,#13275,#13276,#13277,#13278,#13279,#13280,#13281,#13282,
#13283,#13284,#13285,#13286,#13287,#13288,#13289,#13290,#13291,#13292,#13293,
#13294,#13295,#13296,#13297,#13298,#13299,#13300,#13301,#13302,#13303,#13304,
#13305,#13306,#13307,#13308,#13309,#13310,#13311,#13312,#13313,#13314,#13315,
#13316,#13317,#13318,#13319,#13320,#13321,#13322,#13323,#13324,#13325,#13326,
#13327,#13328,#13329,#13330,#13331,#13332,#13333,#13334,#13335,#13336,#13337,
#13338,#13339,#13340,#13341,#13342,#13343,#13344,#13345,#13346,#13347,#13348,
#13349,#13350,#13351,#13352,#13353,#13354,#13355,#13356,#13357,#13358,#13359,
#13360,#13361,#13362,#13363,#13364,#13365,#13366,#13367,#13368,#13369,#13370,
#13371,#13372,#13373,#13374,#13375,#13376,#13377,#13378,#13379,#13380,#13381,
#13382,#13383,#13384,#13385,#13386,#13387,#13388,#13389,#13390,#13391,#13392,
#13393,#13394,#13395,#13396,#13397,#13398,#13399,#13400,#13401,#13402,#13403,
#13404,#13405,#13406,#13407,#13408,#13409,#13410,#13411,#13412,#13413,#13414,
#13415,#13416,#13417,#13418,#13419,#13420,#13421,#13422,#13423,#13424,#13425,
#13426,#13427,#13428,#13429,#13430,#13431,#13432,#13433,#13434,#13435,#13436,
#13437,#13438,#13439,#13440,#13441,#13442,#13443,#13444,#13445,#13446,#13447,
#13448,#13449,#13450,#13451,#13452,#13453,#13454,#13455,#13456,#13457,#13458,
#13459,#13460,#13461,#13462,#13463,#13464,#13465,#13466,#13467,#13468,#13469,
#13470,#13471,#13472,#13473,#13474,#13475,#13476,#13477,#13478,#13479,#13480,
#13481,#13482,#13483,#13484,#13485,#13486,#13487,#13488,#13489,#13490,#13491,
#13492,#13493,#13494,#13495,#13496,#13497,#13498,#13499,#13500,#13501,#13502,
#13503,#13504,#13505,#13506,#13507,#13508,#13509,#13510,#13511,#13512,#13513,
#13514,#13515,#13516,#13517,#13518,#13519,#13520,#13521,#13522,#13523,#13524,
#13525,#13526,#13527,#13528,#13529,#13530,#13531,#13532,#13533,#13534,#13535,
#13536,#13537,#13538,#13539,#13540,#13541,#13542,#13543,#13544,#13545,#13546,
#13547,#13548,#13549,#13550,#13551,#13552,#13553,#13554,#13555,#13556,#13557,
#13558,#13559,#13560,#13561,#13562,#13563,#13564,#13565,#13566,#13567,#13568,
#13569,#13570,#13571,#13572,#13573,#13574,#13575,#13576,#13577,#13578,#13579,
#13580,#13581,#13582,#13583,#13584,#13585,#13586,#13587,#13588,#13589,#13590,
#13591,#13592,#13593,#13594,#13595,#13596),.UNSPECIFIED.,.F.,.F.,(4,3,3,
3,3,3,3,3,3,3,3,3,3,3,3,3,3,3,3,3,3,3,3,3,3,3,3,3,3,3,3,3,3,3,3,3,3,3,3,
3,3,3,3,3,3,3,3,3,3,3,3,3,3,3,3,3,3,3,3,3,3,3,3,3,3,3,3,3,3,3,3,3,3,3,3,
3,3,3,3,3,3,3,3,3,3,3,3,3,3,3,3,3,3,3,3,3,3,3,3,3,3,3,3,3,3,3,3,3,3,3,3,
3,3,3,3,3,3,4),(-22.9424500654772,-22.8507510669165,-22.8432492269214,-22.7550777090342,
-22.743518032141,-22.6599168656772,-22.6431790088504,-22.6114845020791,
-22.6114538130162,-22.5332660091545,-22.525331370706,-22.4393139831972,
-22.3533801271849,-22.288092600173,-22.2675083545179,-22.1955230788735,
-22.1816687380548,-22.0676024323464,-22.0100122996148,-21.9286196934413,
-21.92415681273,-21.838210039868,-21.7522112020671,-21.6727615321577,-21.6660891924192,
-21.6283778145229,-21.6283471254938,-21.5501593170398,-21.5422246798375,
-21.4562072889451,-21.370273429516,-21.3049859330506,-21.2844016534033,
-21.2124163014448,-21.1985620334634,-21.084495727377,-21.0269055880192,
-20.9455126904598,-20.9410500976143,-20.855103321235,-20.7691044799135,
-20.6896548110226,-20.6829824667704,-20.6452711270011,-20.6452404379714,
-20.5670526310498,-20.5591179957949,-20.4731006083946,-20.3871667524656,
-20.3218792629951,-20.3012949798572,-20.2293096167709,-20.215455363415,
-20.1013890607534,-20.0437989249469,-19.9624057597513,-19.9579434380131,
-19.8719966650674,-19.7859978271626,-19.7065481606488,-19.6998758173811,
-19.6621644395034,-19.6621337504489,-19.5839459482762,-19.5760113092192,
-19.4899939227884,-19.4040600678502,-19.338772629847,-19.3181882962524,
-19.246202899276,-19.2323486808462,-19.1182823723598,-19.0606922444959,
-18.979301196102,-18.9748367586413,-18.8888899867884,-18.8028911499858,
-18.7234414782139,-18.716769141311,-18.6790577519268,-18.6790270629265,
-18.6008392476307,-18.5929046099203,-18.5068872116786,-18.4209533449092,
-18.3556657989052,-18.3350815614742,-18.2630962457753,-18.2492419342651,
-18.1351756270659,-18.0775854743959,-17.9961912899178,-17.9917299768508,
-17.905783193446,-17.8197843451551,-17.7403346763732,-17.733662325189,-17.6959510644389,
-17.695920375404,-17.6177325704747,-17.609797943694,-17.5237805667203,-17.4378467211662,
-17.3725591380261,-17.3519749588694,-17.2799897136122,-17.2661353526079,
-17.1520690646227,-17.0944789342378,-17.0130826630226,-17.0086234572,-16.9226766939388,
-16.8366778656107,-16.7572282103778,-16.7505558651585,-16.7128443770544,
-16.7128136878816,-16.6592647585025),.UNSPECIFIED.);
#1420=B_SPLINE_CURVE_WITH_KNOTS('',3,(#13598,#13599,#13600,#13601,#13602,
#13603,#13604,#13605,#13606,#13607,#13608,#13609,#13610,#13611,#13612,#13613,
#13614,#13615,#13616,#13617,#13618,#13619,#13620,#13621,#13622,#13623,#13624,
#13625,#13626,#13627,#13628,#13629,#13630,#13631,#13632,#13633,#13634,#13635,
#13636,#13637,#13638,#13639,#13640,#13641,#13642,#13643,#13644,#13645,#13646,
#13647,#13648,#13649,#13650,#13651,#13652,#13653,#13654,#13655,#13656,#13657,
#13658,#13659,#13660,#13661,#13662,#13663,#13664,#13665,#13666,#13667,#13668,
#13669,#13670,#13671,#13672,#13673,#13674,#13675,#13676,#13677,#13678,#13679,
#13680,#13681,#13682,#13683,#13684,#13685,#13686,#13687,#13688,#13689,#13690,
#13691,#13692,#13693,#13694,#13695,#13696,#13697,#13698,#13699,#13700,#13701,
#13702,#13703,#13704,#13705,#13706,#13707,#13708,#13709,#13710,#13711,#13712,
#13713,#13714,#13715,#13716,#13717,#13718,#13719,#13720,#13721,#13722,#13723,
#13724,#13725,#13726,#13727,#13728,#13729,#13730,#13731,#13732,#13733,#13734,
#13735,#13736,#13737,#13738,#13739,#13740,#13741,#13742,#13743,#13744,#13745,
#13746,#13747,#13748,#13749,#13750,#13751,#13752,#13753,#13754,#13755,#13756,
#13757,#13758,#13759,#13760,#13761,#13762,#13763,#13764,#13765,#13766,#13767,
#13768,#13769,#13770,#13771,#13772,#13773,#13774,#13775,#13776,#13777,#13778,
#13779,#13780,#13781,#13782,#13783,#13784,#13785,#13786,#13787,#13788,#13789,
#13790,#13791,#13792,#13793,#13794,#13795,#13796,#13797,#13798,#13799,#13800,
#13801,#13802,#13803,#13804,#13805,#13806,#13807,#13808,#13809,#13810,#13811,
#13812,#13813,#13814,#13815,#13816,#13817,#13818,#13819,#13820,#13821,#13822,
#13823,#13824,#13825,#13826,#13827,#13828,#13829,#13830,#13831,#13832,#13833,
#13834,#13835,#13836,#13837,#13838,#13839,#13840,#13841,#13842,#13843,#13844,
#13845,#13846,#13847,#13848,#13849,#13850,#13851,#13852,#13853,#13854,#13855,
#13856,#13857,#13858,#13859,#13860,#13861,#13862,#13863,#13864,#13865,#13866,
#13867,#13868,#13869,#13870,#13871,#13872,#13873,#13874,#13875,#13876,#13877,
#13878,#13879,#13880,#13881,#13882,#13883,#13884,#13885,#13886,#13887,#13888,
#13889,#13890,#13891,#13892,#13893,#13894,#13895,#13896,#13897,#13898,#13899,
#13900,#13901,#13902,#13903,#13904,#13905,#13906,#13907,#13908,#13909,#13910,
#13911,#13912,#13913,#13914,#13915,#13916,#13917,#13918,#13919,#13920,#13921,
#13922,#13923,#13924,#13925,#13926,#13927,#13928,#13929,#13930,#13931,#13932,
#13933,#13934,#13935,#13936,#13937),.UNSPECIFIED.,.F.,.F.,(4,3,3,3,3,3,
3,3,3,3,3,3,3,3,3,3,3,3,3,3,3,3,3,3,3,3,3,3,3,3,3,3,3,3,3,3,3,3,3,3,3,3,
3,3,3,3,3,3,3,3,3,3,3,3,3,3,3,3,3,3,3,3,3,3,3,3,3,3,3,3,3,3,3,3,3,3,3,3,
3,3,3,3,3,3,3,3,3,3,3,3,3,3,3,3,3,3,3,3,3,3,3,3,3,3,3,3,3,3,3,3,3,3,3,4),
(-16.6592647583439,-16.57834727546,-16.5738430149373,-16.4885227334712,
-16.4032816523275,-16.3459598776537,-16.3180945864984,-16.2004506632273,
-16.1477847574117,-16.0817816596509,-16.0626219831902,-15.9942979489986,
-15.9773761668429,-15.8920884458071,-15.8066680671297,-15.7297376890762,
-15.7297070003591,-15.651519114883,-15.6435844798867,-15.5575670140271,
-15.471633079569,-15.4063449429491,-15.3857612284546,-15.3137763848075,
-15.2999215338279,-15.1858552272951,-15.1282649397453,-15.0468548409394,
-15.0424093755484,-14.9564625263443,-14.8704636126523,-14.7910139547004,
-14.7843415284612,-14.7466310020105,-14.7466003128367,-14.6684125526381,
-14.6604779921827,-14.5744607260426,-14.4885269909739,-14.4232390313135,
-14.4026553386888,-14.3306706437354,-14.3168158413389,-14.2027496692409,
-14.145159638529,-14.0637467865836,-14.0593042679126,-13.9733576090808,
-13.8873588841852,-13.8079093131886,-13.8012369847486,-13.7635243153496,
-13.7634936253142,-13.685306041895,-13.6773712241262,-13.5913538790123,
-13.5054200666001,-13.4401363550069,-13.4195483386733,-13.3475593369649,
-13.3337087684636,-13.2196421674157,-13.162052425251,-13.0807773831844,
-13.0761969872289,-12.99025026418,-12.9042514768019,-12.8248015432038,-12.8181295180617,
-12.7804176239796,-12.7803869377918,-12.7021984322804,-12.6942638863894,
-12.6082458879433,-12.5223114198845,-12.457017353168,-12.4364390347946,
-12.3644591608565,-12.3505988075939,-12.2365326173997,-12.1789411520357,
-12.0930850600792,-12.0071376892478,-11.9211382567276,-11.8416887815353,
-11.8350156624911,-11.7973109415761,-11.7972802502693,-11.719093095323,
-11.7111590060667,-11.6251428153763,-11.5392101535174,-11.4739218216529,
-11.4533395709698,-11.3813569797693,-11.367501134333,-11.2534358016061,
-11.195847034049,-11.1143771280478,-11.1099927030158,-11.0240470659038,
-10.9380493539021,-10.858600351834,-10.851928445109,-10.8142042584984,-10.8141735627469,
-10.7330908037065,-10.7213212232863,-10.6350324102581,-10.6287599994176,
-10.5363786705168,-10.4732766489798,-10.4442738471014,-10.3760794514417),
 .UNSPECIFIED.);
#1421=B_SPLINE_CURVE_WITH_KNOTS('',3,(#13938,#13939,#13940,#13941,#13942,
#13943,#13944,#13945,#13946,#13947,#13948,#13949,#13950,#13951,#13952,#13953,
#13954,#13955,#13956,#13957,#13958,#13959,#13960,#13961,#13962,#13963,#13964,
#13965,#13966,#13967,#13968,#13969,#13970,#13971,#13972,#13973,#13974,#13975,
#13976,#13977,#13978,#13979,#13980,#13981,#13982,#13983,#13984,#13985,#13986,
#13987,#13988,#13989,#13990,#13991,#13992,#13993,#13994,#13995,#13996,#13997,
#13998,#13999,#14000,#14001,#14002,#14003,#14004,#14005,#14006,#14007,#14008,
#14009,#14010,#14011,#14012,#14013,#14014,#14015,#14016,#14017,#14018,#14019,
#14020,#14021,#14022,#14023,#14024,#14025,#14026,#14027,#14028,#14029,#14030,
#14031,#14032,#14033,#14034,#14035,#14036,#14037,#14038,#14039,#14040,#14041,
#14042,#14043,#14044,#14045,#14046,#14047,#14048,#14049,#14050,#14051,#14052,
#14053,#14054,#14055,#14056,#14057,#14058,#14059,#14060,#14061,#14062,#14063,
#14064,#14065,#14066,#14067,#14068,#14069,#14070,#14071,#14072,#14073,#14074,
#14075,#14076,#14077,#14078,#14079,#14080,#14081,#14082,#14083,#14084,#14085,
#14086,#14087,#14088,#14089,#14090,#14091,#14092,#14093,#14094,#14095,#14096,
#14097,#14098,#14099,#14100,#14101,#14102,#14103,#14104,#14105,#14106,#14107,
#14108,#14109,#14110,#14111,#14112,#14113,#14114,#14115,#14116,#14117,#14118,
#14119,#14120,#14121,#14122,#14123,#14124,#14125,#14126,#14127,#14128,#14129,
#14130,#14131,#14132,#14133,#14134,#14135,#14136,#14137,#14138,#14139,#14140,
#14141,#14142,#14143,#14144,#14145,#14146,#14147,#14148,#14149,#14150,#14151,
#14152,#14153,#14154,#14155,#14156,#14157,#14158,#14159,#14160,#14161,#14162,
#14163,#14164,#14165,#14166,#14167,#14168,#14169,#14170,#14171,#14172,#14173,
#14174,#14175,#14176,#14177,#14178,#14179,#14180,#14181,#14182,#14183,#14184,
#14185,#14186,#14187,#14188,#14189,#14190,#14191,#14192,#14193,#14194,#14195,
#14196,#14197,#14198,#14199,#14200,#14201,#14202,#14203,#14204,#14205,#14206,
#14207,#14208,#14209,#14210,#14211,#14212,#14213,#14214,#14215,#14216,#14217,
#14218,#14219,#14220,#14221,#14222,#14223,#14224,#14225,#14226,#14227,#14228,
#14229,#14230,#14231,#14232,#14233,#14234,#14235,#14236,#14237,#14238,#14239,
#14240,#14241,#14242,#14243,#14244,#14245,#14246,#14247,#14248,#14249,#14250,
#14251,#14252,#14253,#14254,#14255,#14256,#14257,#14258,#14259,#14260,#14261,
#14262,#14263,#14264,#14265,#14266,#14267,#14268,#14269,#14270,#14271,#14272,
#14273,#14274,#14275,#14276,#14277,#14278,#14279,#14280),.UNSPECIFIED.,
 .F.,.F.,(4,3,3,3,3,3,3,3,3,3,3,3,3,3,3,3,3,3,3,3,3,3,3,3,3,3,3,3,3,3,3,
3,3,3,3,3,3,3,3,3,3,3,3,3,3,3,3,3,3,3,3,3,3,3,3,3,3,3,3,3,3,3,3,3,3,3,3,
3,3,3,3,3,3,3,3,3,3,3,3,3,3,3,3,3,3,3,3,3,3,3,3,3,3,3,3,3,3,3,3,3,3,3,3,
3,3,3,3,3,3,3,3,3,3,3,4),(-10.3760794513229,-10.3264153263384,-10.2925120173749,
-10.2601968567228,-10.1998923966073,-10.1363908395232,-10.1076860162616,
-10.0193432467952,-9.93091491142239,-9.85194692512929,-9.84233871959151,
-9.83109753959046,-9.83106687522445,-9.75287310045053,-9.74493984606962,
-9.65891785327206,-9.57297937914544,-9.50762889976171,-9.48710298111784,
-9.41517189571804,-9.40125874556535,-9.28719446135969,-9.22959308987034,
-9.14373301477612,-9.05778170156634,-8.97177834463815,-8.89233113759898,
-8.88565188756136,-8.84799090459512,-8.84796018770201,-8.76977990021687,
-8.76184887755315,-8.67584262021201,-8.58991987947197,-8.52465246550391,
-8.50405919433414,-8.43207207388185,-8.41823058404444,-8.30417088660895,
-8.24659598478001,-8.16537366735408,-8.16075130772062,-8.07481517058394,
-7.98882688343906,-7.90938128579593,-7.90271520305529,-7.86488422895974,
-7.86485350017956,-7.78667353382456,-7.77872495169094,-7.69270153910995,
-7.60676174503123,-7.54168886120423,-7.52088412724879,-7.44867448273856,
-7.4350388238479,-7.32094923965079,-7.26337131704426,-7.18787402876446,
-7.17751045990625,-7.09155851220294,-7.00555460422482,-6.92608545369845,
-6.91942772756424,-6.88177729574692,-6.88174681265712,-6.80350986483478,
-6.79559175471683,-6.70954157508135,-6.62357479127157,-6.55770110774451,
-6.53766999564482,-6.46618696034968,-6.45179733750838,-6.33775687888313,
-6.2800748480303,-6.19418642384597,-6.10820699948371,-6.02217562967714,
-5.94275307736442,-5.936021553422,-5.89867111508928,-5.89864012513467,-5.82053057812116,
-5.8126166075868,-5.72669820066755,-5.64086326704925,-5.57596685375035,
-5.55509024515823,-5.48287344868061,-5.46934876919013,-5.35532269157411,
-5.2978872897214,-5.22328485573253,-5.21212841716633,-5.12627681995917,
-5.04037246723583,-4.96094257333632,-4.95434306467912,-4.91556430437963,
-4.91553343761223,-4.83814842128407,-4.83052634717772,-4.74562463000397,
-4.66081596132364,-4.59544057673657,-4.57605895127486,-4.50694700115561,
-4.49133320716937,-4.37135018659226,-4.32185837814588,-4.26407962449433,
-4.23707535482957,-4.15219887483577,-4.09289414427507),.UNSPECIFIED.);
#1422=B_SPLINE_CURVE_WITH_KNOTS('',3,(#14307,#14308,#14309,#14310,#14311,
#14312,#14313,#14314,#14315,#14316,#14317,#14318,#14319,#14320,#14321,#14322,
#14323,#14324,#14325,#14326,#14327,#14328,#14329,#14330,#14331,#14332,#14333,
#14334,#14335,#14336,#14337,#14338,#14339,#14340,#14341,#14342,#14343,#14344,
#14345,#14346,#14347,#14348,#14349,#14350,#14351,#14352,#14353,#14354,#14355,
#14356,#14357,#14358,#14359,#14360,#14361,#14362,#14363,#14364,#14365,#14366,
#14367,#14368,#14369,#14370,#14371,#14372,#14373,#14374,#14375,#14376,#14377,
#14378,#14379,#14380,#14381,#14382,#14383,#14384,#14385,#14386,#14387,#14388,
#14389,#14390,#14391,#14392,#14393,#14394),.UNSPECIFIED.,.F.,.F.,(4,3,3,
3,3,3,3,3,3,3,3,3,3,3,3,3,3,3,3,3,3,3,3,3,3,3,3,3,3,4),(2.05878368674717E-14,
0.0234054472019564,0.0471352136142213,0.0707669153608998,0.0840367480408261,
0.0878713467795278,0.110975706690514,0.133712282260844,0.150709160734639,
0.158060268187143,0.163470733062873,0.167953178850733,0.189907599318317,
0.201793217244577,0.224252520140966,0.234752288110081,0.240507487537732,
0.24411168274315,0.265884710195976,0.287663355668543,0.308957241466627,
0.317294467212432,0.321188873214287,0.341934990903991,0.362478952452641,
0.367608141617428,0.372096895882347,0.385217611626515,0.405963257765431,
0.415993328865176),.UNSPECIFIED.);
#1423=B_SPLINE_CURVE_WITH_KNOTS('',3,(#14396,#14397,#14398,#14399),
 .UNSPECIFIED.,.F.,.F.,(4,4),(-2.84914982550175,-2.06894047480313),
 .UNSPECIFIED.);
#1424=B_SPLINE_CURVE_WITH_KNOTS('',3,(#14401,#14402,#14403,#14404,#14405,
#14406,#14407,#14408,#14409,#14410,#14411,#14412,#14413,#14414,#14415,#14416,
#14417,#14418,#14419,#14420,#14421,#14422,#14423,#14424,#14425,#14426,#14427,
#14428,#14429,#14430,#14431,#14432,#14433,#14434,#14435,#14436,#14437,#14438,
#14439,#14440,#14441,#14442,#14443,#14444,#14445,#14446,#14447,#14448,#14449,
#14450,#14451,#14452,#14453,#14454,#14455,#14456,#14457,#14458,#14459,#14460,
#14461,#14462,#14463,#14464,#14465,#14466,#14467,#14468,#14469,#14470,#14471,
#14472,#14473,#14474,#14475,#14476,#14477,#14478,#14479,#14480,#14481,#14482,
#14483,#14484,#14485,#14486,#14487,#14488),.UNSPECIFIED.,.F.,.F.,(4,3,3,
3,3,3,3,3,3,3,3,3,3,3,3,3,3,3,3,3,3,3,3,3,3,3,3,3,3,4),(-0.413490722097494,
-0.390374461965417,-0.376956788739721,-0.364612854506389,-0.357223081629536,
-0.353167632297454,-0.329816475302324,-0.3110173587975,-0.300922997939596,
-0.297410089408388,-0.274622870919242,-0.252197899216542,-0.232987043189295,
-0.22435563742345,-0.220563464855743,-0.216970640358496,-0.195389510666055,
-0.179453841006409,-0.15736082632792,-0.146597972574468,-0.141428288189789,
-0.120027659580677,-0.0986007772958362,-0.077592352147286,-0.0725581786302476,
-0.0680299217253234,-0.0474235785525696,-0.0274062962751784,-0.00761976281229705,
0.),.UNSPECIFIED.);
#1425=B_SPLINE_CURVE_WITH_KNOTS('',3,(#14490,#14491,#14492,#14493,#14494,
#14495,#14496,#14497),.UNSPECIFIED.,.F.,.F.,(4,2,2,4),(-0.139393279070508,
-0.0696441449762668,-0.0347017080904481,-0.000337482562019728),
 .UNSPECIFIED.);
#1426=B_SPLINE_CURVE_WITH_KNOTS('',3,(#14498,#14499,#14500,#14501),
 .UNSPECIFIED.,.F.,.F.,(4,4),(-0.00186151085722638,0.),.UNSPECIFIED.);
#1427=B_SPLINE_CURVE_WITH_KNOTS('',3,(#14506,#14507,#14508,#14509,#14510,
#14511,#14512,#14513),.UNSPECIFIED.,.F.,.F.,(4,2,2,4),(0.000337254956516375,
0.0347017162006212,0.0696441548061046,0.139393290074209),.UNSPECIFIED.);
#1428=B_SPLINE_CURVE_WITH_KNOTS('',3,(#14540,#14541,#14542,#14543,#14544,
#14545,#14546,#14547,#14548,#14549,#14550,#14551,#14552,#14553,#14554,#14555,
#14556,#14557,#14558,#14559,#14560,#14561,#14562,#14563,#14564,#14565,#14566,
#14567,#14568,#14569,#14570,#14571,#14572,#14573,#14574,#14575,#14576,#14577,
#14578,#14579,#14580,#14581,#14582,#14583,#14584,#14585,#14586,#14587,#14588,
#14589,#14590,#14591,#14592,#14593,#14594,#14595,#14596,#14597,#14598,#14599,
#14600,#14601,#14602,#14603,#14604,#14605,#14606,#14607,#14608,#14609,#14610,
#14611,#14612,#14613,#14614,#14615,#14616,#14617,#14618,#14619,#14620,#14621,
#14622,#14623,#14624,#14625,#14626,#14627),.UNSPECIFIED.,.F.,.F.,(4,3,3,
3,3,3,3,3,3,3,3,3,3,3,3,3,3,3,3,3,3,3,3,3,3,3,3,3,3,4),(9.94883000103285E-15,
0.0196166916569847,0.0399302769784652,0.0573080150775109,0.0651965825194071,
0.0692472851263457,0.0727586240116996,0.0938497532114967,0.115302615032433,
0.136627386511764,0.139448576973331,0.143452860461702,0.147424687779491,
0.169517815215389,0.179453841006421,0.2010748625388,0.220290031668888,0.22390552179017,
0.245971799153012,0.26870301781468,0.291434236476348,0.297317452472671,
0.303372200521482,0.326746258433795,0.349433290040221,0.355210854434181,
0.360866724042728,0.37695678873974,0.400080606860445,0.414094136780462),
 .UNSPECIFIED.);
#1429=B_SPLINE_CURVE_WITH_KNOTS('',3,(#14629,#14630,#14631,#14632),
 .UNSPECIFIED.,.F.,.F.,(4,4),(0.,0.00186027720717915),.UNSPECIFIED.);
#1430=B_SPLINE_CURVE_WITH_KNOTS('',3,(#14634,#14635,#14636,#14637,#14638,
#14639,#14640,#14641,#14642,#14643,#14644,#14645,#14646,#14647,#14648,#14649,
#14650,#14651,#14652,#14653,#14654,#14655,#14656,#14657,#14658,#14659,#14660,
#14661,#14662,#14663,#14664,#14665,#14666,#14667,#14668,#14669,#14670,#14671,
#14672,#14673,#14674,#14675,#14676,#14677,#14678,#14679,#14680,#14681,#14682,
#14683,#14684,#14685,#14686,#14687,#14688,#14689,#14690,#14691,#14692,#14693,
#14694,#14695,#14696,#14697,#14698,#14699,#14700,#14701,#14702,#14703,#14704,
#14705,#14706,#14707,#14708,#14709,#14710,#14711,#14712,#14713,#14714,#14715),
 .UNSPECIFIED.,.F.,.F.,(4,3,3,3,3,3,3,3,3,3,3,3,3,3,3,3,3,3,3,3,3,3,3,3,
3,3,3,4),(-0.415993328865187,-0.395247681143785,-0.385217611626505,-0.368797025934534,
-0.36502116844561,-0.344384137832406,-0.326531494809057,-0.320844694700121,
-0.315794800692042,-0.294447216736322,-0.272640318795181,-0.255006113686598,
-0.246851849353904,-0.243114662305886,-0.220650412226071,-0.201793217244566,
-0.179843818695368,-0.168406146924892,-0.164760369659269,-0.142479944943098,
-0.119441369865257,-0.0964027947874157,-0.086570173338417,-0.0816436307916124,
-0.0579861482246397,-0.0343081270343868,-0.0108824362787603,0.),
 .UNSPECIFIED.);
#1431=B_SPLINE_CURVE_WITH_KNOTS('',3,(#14716,#14717,#14718,#14719),
 .UNSPECIFIED.,.F.,.F.,(4,4),(0.,0.780209350698613),.UNSPECIFIED.);
#1432=B_SPLINE_CURVE_WITH_KNOTS('',3,(#14921,#14922,#14923,#14924,#14925,
#14926,#14927,#14928,#14929,#14930,#14931,#14932,#14933,#14934,#14935,#14936,
#14937,#14938,#14939,#14940,#14941,#14942,#14943,#14944,#14945,#14946,#14947,
#14948,#14949,#14950,#14951,#14952,#14953,#14954,#14955,#14956,#14957,#14958,
#14959,#14960,#14961,#14962,#14963,#14964,#14965,#14966,#14967,#14968,#14969,
#14970,#14971,#14972,#14973,#14974,#14975,#14976,#14977,#14978,#14979,#14980,
#14981,#14982,#14983,#14984,#14985,#14986,#14987,#14988,#14989,#14990,#14991,
#14992,#14993,#14994,#14995,#14996,#14997,#14998,#14999,#15000,#15001,#15002,
#15003,#15004,#15005,#15006,#15007,#15008,#15009,#15010,#15011,#15012,#15013,
#15014,#15015,#15016,#15017,#15018,#15019,#15020,#15021,#15022,#15023,#15024,
#15025,#15026),.UNSPECIFIED.,.F.,.F.,(4,3,3,3,3,3,3,3,3,3,3,3,3,3,3,3,3,
3,3,3,3,3,3,3,3,3,3,3,3,3,3,3,3,3,3,4),(5.51919316556669E-5,0.0396105854411369,
0.0421684740053724,0.0820591227434645,0.123381779682084,0.164704436620703,
0.170094771591715,0.175319647983374,0.214784946467128,0.25429154179183,
0.293151938457061,0.325136464664712,0.334844260977463,0.340168266397053,
0.37840317841123,0.416167211420586,0.452998512977425,0.46134294969662,0.485996360447615,
0.493345060083779,0.499697573685857,0.536831195961491,0.574162340000071,
0.61108256799235,0.632520778240444,0.644430130512825,0.650618647569442,
0.655220962152611,0.658570235704578,0.695166161482855,0.731571524858071,
0.744958227452224,0.754067922795179,0.789881274989443,0.825088562680887,
0.847325527525853),.UNSPECIFIED.);
#1433=B_SPLINE_CURVE_WITH_KNOTS('',3,(#15028,#15029,#15030,#15031,#15032,
#15033,#15034,#15035,#15036,#15037,#15038,#15039,#15040,#15041,#15042,#15043,
#15044,#15045,#15046,#15047,#15048,#15049,#15050,#15051,#15052,#15053,#15054,
#15055,#15056,#15057,#15058,#15059,#15060,#15061,#15062,#15063,#15064,#15065,
#15066,#15067,#15068,#15069,#15070,#15071,#15072,#15073,#15074,#15075,#15076,
#15077,#15078,#15079,#15080,#15081,#15082,#15083,#15084,#15085,#15086,#15087,
#15088,#15089,#15090,#15091,#15092,#15093,#15094,#15095,#15096,#15097,#15098,
#15099,#15100,#15101,#15102,#15103,#15104,#15105,#15106,#15107,#15108,#15109,
#15110,#15111,#15112,#15113,#15114,#15115,#15116,#15117,#15118,#15119,#15120,
#15121,#15122,#15123,#15124),.UNSPECIFIED.,.F.,.F.,(4,3,3,3,3,3,3,3,3,3,
3,3,3,3,3,3,3,3,3,3,3,3,3,3,3,3,3,3,3,3,3,3,4),(-0.847325527525843,-0.811503753623457,
-0.776673059854492,-0.75974088209237,-0.750234800273659,-0.742631895672967,
-0.706740314620834,-0.670224472629315,-0.65436706634716,-0.6449569526527,
-0.607798067978851,-0.570230375047688,-0.532703103593353,-0.505758215660538,
-0.497488333365585,-0.491961441323387,-0.453421092889369,-0.422238544386844,
-0.384505330263272,-0.346772116139701,-0.33539303508032,-0.33016070262821,
-0.291919157074523,-0.252839602008931,-0.215142387780448,-0.175907489429898,
-0.170455452500928,-0.156701908810693,-0.116751637160037,-0.0766037057486563,
-0.0367647523419657,-0.00225557790275668,-1.20338083946995E-14),
 .UNSPECIFIED.);
#1434=B_SPLINE_CURVE_WITH_KNOTS('',3,(#15125,#15126,#15127,#15128),
 .UNSPECIFIED.,.F.,.F.,(4,4),(-0.00895779246149321,0.),.UNSPECIFIED.);
#1435=B_SPLINE_CURVE_WITH_KNOTS('',3,(#15322,#15323,#15324,#15325,#15326,
#15327,#15328,#15329,#15330,#15331,#15332,#15333,#15334,#15335,#15336,#15337,
#15338,#15339,#15340,#15341,#15342,#15343,#15344,#15345,#15346,#15347,#15348,
#15349,#15350,#15351,#15352,#15353,#15354,#15355,#15356,#15357,#15358,#15359,
#15360,#15361,#15362,#15363,#15364,#15365,#15366,#15367,#15368,#15369,#15370,
#15371,#15372,#15373,#15374,#15375,#15376,#15377,#15378,#15379,#15380,#15381,
#15382,#15383,#15384,#15385,#15386,#15387,#15388,#15389,#15390,#15391,#15392,
#15393,#15394,#15395,#15396,#15397,#15398,#15399,#15400,#15401,#15402,#15403,
#15404,#15405,#15406,#15407,#15408,#15409,#15410,#15411,#15412,#15413,#15414,
#15415,#15416,#15417,#15418),.UNSPECIFIED.,.F.,.F.,(4,3,3,3,3,3,3,3,3,3,
3,3,3,3,3,3,3,3,3,3,3,3,3,3,3,3,3,3,3,3,3,3,4),(0.,0.0357326537857237,0.0704068465260574,
0.106060821374739,0.14171479622342,0.147192652306303,0.152214352689264,
0.188520307438454,0.225451162932226,0.262649253600598,0.282094339758411,
0.294929882792059,0.30572005862029,0.343770262441978,0.381690975206976,
0.418209942863103,0.423963173602016,0.455960576699411,0.461085295912164,
0.499207673622447,0.537393570095102,0.576100145693367,0.613574806753294,
0.619086816026134,0.624483039944413,0.630147733446615,0.669254131242952,
0.708784888661744,0.727582209613668,0.735557703752757,0.775673392218803,
0.815702463241756,0.84421229055669),.UNSPECIFIED.);
#1436=B_SPLINE_CURVE_WITH_KNOTS('',3,(#15419,#15420,#15421,#15422),
 .UNSPECIFIED.,.F.,.F.,(4,4),(0.,0.00895786573059968),.UNSPECIFIED.);
#1437=B_SPLINE_CURVE_WITH_KNOTS('',3,(#15423,#15424,#15425,#15426,#15427,
#15428,#15429,#15430,#15431,#15432,#15433,#15434,#15435,#15436,#15437,#15438,
#15439,#15440,#15441,#15442,#15443,#15444,#15445,#15446,#15447,#15448,#15449,
#15450,#15451,#15452,#15453,#15454,#15455,#15456,#15457,#15458,#15459,#15460,
#15461,#15462,#15463,#15464,#15465,#15466,#15467,#15468,#15469,#15470,#15471,
#15472,#15473,#15474,#15475,#15476,#15477,#15478,#15479,#15480,#15481,#15482,
#15483,#15484,#15485,#15486,#15487,#15488,#15489,#15490,#15491,#15492,#15493,
#15494,#15495,#15496,#15497,#15498,#15499,#15500,#15501,#15502,#15503,#15504,
#15505,#15506,#15507,#15508,#15509,#15510,#15511,#15512,#15513,#15514,#15515,
#15516,#15517,#15518,#15519),.UNSPECIFIED.,.F.,.F.,(4,3,3,3,3,3,3,3,3,3,
3,3,3,3,3,3,3,3,3,3,3,3,3,3,3,3,3,3,3,3,3,3,4),(-0.844212290556731,-0.804914039435832,
-0.802217933301225,-0.761940655968895,-0.731371284183562,-0.724667747997382,
-0.685031612040754,-0.645191108298448,-0.631145243959577,-0.622466655133243,
-0.614790169492861,-0.575736023750926,-0.536900490369521,-0.498311999539644,
-0.459723508709767,-0.457469136431715,-0.452285602603943,-0.414914580184266,
-0.385002433230672,-0.347245920152347,-0.309123322414732,-0.301425288615579,
-0.29421526181017,-0.257399270414763,-0.220741128783992,-0.188385367654945,
-0.153950864306229,-0.147824231453246,-0.142510002622108,-0.106551008291469,
-0.0707579690466674,-0.0353789845233405,-1.35445026026053E-14),
 .UNSPECIFIED.);
#1438=B_SPLINE_CURVE_WITH_KNOTS('',3,(#15546,#15547,#15548,#15549,#15550,
#15551,#15552,#15553,#15554,#15555,#15556,#15557,#15558,#15559,#15560,#15561,
#15562,#15563,#15564,#15565,#15566,#15567,#15568,#15569,#15570,#15571),
 .UNSPECIFIED.,.F.,.F.,(4,2,2,2,2,2,2,2,2,2,2,2,4),(-0.606481282784619,
-0.568571286664201,-0.530661290543783,-0.492761126316124,-0.454860962088464,
-0.416960797860805,-0.379060633633146,-0.341150637512728,-0.30324064139231,
-0.265330645271891,-0.227420649151473,-0.189520484923814,-0.151620320696155),
 .UNSPECIFIED.);
#1439=B_SPLINE_CURVE_WITH_KNOTS('',3,(#15572,#15573,#15574,#15575,#15576,
#15577,#15578,#15579,#15580,#15581),.UNSPECIFIED.,.F.,.F.,(4,2,2,2,4),(-0.151620320696155,
-0.113720156468496,-0.0758199922408364,-0.0379099961204182,0.),
 .UNSPECIFIED.);
#1440=B_SPLINE_CURVE_WITH_KNOTS('',3,(#15585,#15586,#15587,#15588,#15589,
#15590,#15591,#15592,#15593,#15594),.UNSPECIFIED.,.F.,.F.,(4,2,2,2,4),(0.,
0.0377168406459521,0.0754336812919042,0.113150118256495,0.150866555221085),
 .UNSPECIFIED.);
#1441=B_SPLINE_CURVE_WITH_KNOTS('',3,(#15595,#15596,#15597,#15598,#15599,
#15600,#15601,#15602,#15603,#15604,#15605,#15606,#15607,#15608,#15609,#15610,
#15611,#15612,#15613,#15614,#15615,#15616,#15617,#15618,#15619,#15620),
 .UNSPECIFIED.,.F.,.F.,(4,2,2,2,2,2,2,2,2,2,2,2,4),(0.150866555221085,0.188582992185676,
0.226299429150267,0.264016269796219,0.301733110442171,0.339449951088123,
0.377166791734075,0.414883228698666,0.452599665663256,0.490316102627847,
0.528032539592437,0.565749380238389,0.603466220884342),.UNSPECIFIED.);
#1442=B_SPLINE_CURVE_WITH_KNOTS('',3,(#15724,#15725,#15726,#15727),
 .UNSPECIFIED.,.F.,.F.,(4,4),(2.77524983164141,2.7754356884636),
 .UNSPECIFIED.);
#1443=B_SPLINE_CURVE_WITH_KNOTS('',3,(#15729,#15730,#15731,#15732,#15733,
#15734,#15735,#15736,#15737,#15738,#15739,#15740,#15741,#15742,#15743,#15744,
#15745,#15746,#15747,#15748,#15749,#15750,#15751,#15752,#15753,#15754,#15755,
#15756,#15757,#15758,#15759,#15760,#15761,#15762,#15763,#15764,#15765,#15766,
#15767,#15768,#15769,#15770,#15771,#15772,#15773,#15774,#15775,#15776,#15777,
#15778,#15779,#15780,#15781,#15782,#15783,#15784,#15785,#15786,#15787,#15788,
#15789,#15790,#15791,#15792,#15793,#15794,#15795,#15796,#15797,#15798,#15799,
#15800,#15801,#15802,#15803,#15804,#15805,#15806,#15807,#15808,#15809,#15810,
#15811,#15812,#15813,#15814,#15815,#15816,#15817,#15818,#15819,#15820,#15821,
#15822,#15823,#15824,#15825,#15826,#15827,#15828,#15829,#15830,#15831,#15832,
#15833,#15834,#15835,#15836,#15837,#15838,#15839,#15840,#15841,#15842,#15843,
#15844,#15845,#15846,#15847,#15848,#15849,#15850,#15851,#15852),
 .UNSPECIFIED.,.F.,.F.,(4,3,3,3,3,3,3,3,3,3,3,3,3,3,3,3,3,3,3,3,3,3,3,3,
3,3,3,3,3,3,3,3,3,3,3,3,3,3,3,3,3,4),(-5.2891562906822,-5.18360776201043,
-5.16592202403009,-5.06502794865638,-5.0409071101405,-4.991013367524,-4.99097352154249,
-4.89791297254004,-4.8887207823386,-4.78661873310371,-4.68463617498642,
-4.58271830049947,-4.48083193862712,-4.37894396049634,-4.27695022114797,
-4.17490252616154,-4.07267004030852,-3.9928178800891,-3.99277881723399,
-3.89952340746646,-3.89022667007414,-3.78782539108402,-3.68554527959923,
-3.58333102513057,-3.48114986928111,-3.37896909715953,-3.27668767666928,
-3.17435468887112,-3.0718440432757,-2.9946218545813,-2.99458411292549,-2.90179614365268,
-2.89325038855348,-2.79021171641803,-2.68914057287426,-2.58812832611143,
-2.48714069765389,-2.38259077610789,-2.28148996903811,-2.175215490254,-2.07915882623621,
-2.06894888197497),.UNSPECIFIED.);
#1444=B_SPLINE_CURVE_WITH_KNOTS('',3,(#15854,#15855,#15856,#15857,#15858,
#15859),.UNSPECIFIED.,.F.,.F.,(4,2,4),(0.000102523276221914,0.00211374109474727,
0.00412550342438516),.UNSPECIFIED.);
#1445=B_SPLINE_CURVE_WITH_KNOTS('',3,(#15867,#15868,#15869,#15870,#15871,
#15872,#15873,#15874,#15875,#15876,#15877,#15878,#15879,#15880,#15881,#15882,
#15883,#15884,#15885,#15886,#15887,#15888,#15889,#15890,#15891,#15892,#15893,
#15894,#15895,#15896,#15897,#15898,#15899,#15900,#15901,#15902,#15903,#15904,
#15905,#15906,#15907,#15908,#15909,#15910,#15911,#15912,#15913,#15914,#15915,
#15916,#15917,#15918,#15919,#15920,#15921,#15922,#15923,#15924,#15925,#15926,
#15927,#15928,#15929,#15930,#15931,#15932,#15933,#15934,#15935,#15936),
 .UNSPECIFIED.,.F.,.F.,(4,3,3,3,3,3,3,3,3,3,3,3,3,3,3,3,3,3,3,3,3,3,3,4),
(0.,0.104661171317195,0.209255039882458,0.313836025669164,0.418414672909222,
0.523017976486558,0.627672951902333,0.732486530385716,0.837386576506837,
0.942488701205836,0.998194704308485,1.09966450843524,1.20096987785232,1.30213869551464,
1.40323263958923,1.50428592829615,1.60533272568538,1.70647828415392,1.80767242300264,
1.9090522202859,1.99638940861699,2.12019797963207,2.24242280953419,2.31370279205594),
 .UNSPECIFIED.);
#1446=B_SPLINE_CURVE_WITH_KNOTS('',3,(#15939,#15940,#15941,#15942,#15943,
#15944,#15945,#15946,#15947,#15948),.UNSPECIFIED.,.F.,.F.,(4,2,2,2,4),(0.,
0.038320218022911,0.076640436045822,0.114893233564743,0.153146031083664),
 .UNSPECIFIED.);
#1447=B_SPLINE_CURVE_WITH_KNOTS('',3,(#15949,#15950,#15951,#15952,#15953,
#15954,#15955,#15956,#15957,#15958,#15959,#15960,#15961,#15962,#15963,#15964,
#15965,#15966,#15967,#15968,#15969,#15970,#15971,#15972,#15973,#15974),
 .UNSPECIFIED.,.F.,.F.,(4,2,2,2,2,2,2,2,2,2,2,2,4),(0.153146031083664,0.191398828602585,
0.229651626121507,0.267971844144418,0.306292062167329,0.344612280190239,
0.382932498213151,0.421185295732072,0.459438093250993,0.497690890769914,
0.535943688288835,0.574263906311746,0.612584124334657),.UNSPECIFIED.);
#1448=B_SPLINE_CURVE_WITH_KNOTS('',3,(#15979,#15980,#15981,#15982,#15983,
#15984,#15985,#15986,#15987,#15988,#15989,#15990,#15991,#15992,#15993,#15994,
#15995,#15996,#15997,#15998,#15999,#16000,#16001,#16002,#16003,#16004,#16005,
#16006,#16007,#16008,#16009,#16010,#16011,#16012,#16013,#16014,#16015,#16016,
#16017,#16018,#16019,#16020,#16021,#16022,#16023,#16024,#16025,#16026,#16027,
#16028,#16029,#16030,#16031,#16032,#16033,#16034,#16035,#16036,#16037,#16038,
#16039,#16040,#16041,#16042,#16043,#16044,#16045,#16046,#16047,#16048,#16049,
#16050,#16051,#16052,#16053,#16054,#16055,#16056,#16057,#16058,#16059,#16060,
#16061,#16062,#16063,#16064,#16065,#16066,#16067,#16068,#16069,#16070,#16071,
#16072,#16073,#16074,#16075,#16076,#16077,#16078,#16079,#16080,#16081,#16082,
#16083,#16084,#16085,#16086,#16087,#16088,#16089,#16090,#16091,#16092,#16093,
#16094,#16095,#16096,#16097,#16098,#16099,#16100,#16101,#16102,#16103,#16104,
#16105,#16106,#16107,#16108,#16109,#16110,#16111,#16112,#16113,#16114,#16115,
#16116,#16117,#16118,#16119,#16120,#16121,#16122,#16123,#16124,#16125,#16126,
#16127,#16128,#16129,#16130,#16131,#16132,#16133,#16134,#16135,#16136,#16137,
#16138,#16139,#16140,#16141,#16142,#16143,#16144,#16145,#16146,#16147,#16148,
#16149,#16150,#16151,#16152,#16153,#16154,#16155,#16156,#16157,#16158,#16159,
#16160,#16161,#16162,#16163,#16164,#16165,#16166,#16167,#16168,#16169,#16170,
#16171,#16172,#16173,#16174,#16175,#16176,#16177,#16178,#16179,#16180,#16181,
#16182,#16183,#16184,#16185,#16186,#16187,#16188),.UNSPECIFIED.,.F.,.F.,
(4,2,2,2,2,2,2,2,2,2,2,2,2,2,2,2,2,2,2,2,2,2,2,2,2,2,2,2,2,2,2,2,2,2,2,
2,2,2,2,2,2,2,2,2,2,2,2,2,2,2,2,2,2,2,2,2,2,2,2,2,2,2,2,2,2,2,2,2,2,2,2,
2,2,2,2,2,2,2,2,2,2,2,2,2,2,2,2,2,2,2,2,2,2,2,2,2,2,2,2,2,2,2,2,2,4),(1.38781753873472,
1.39967307302691,1.40445914459052,1.40800356043637,1.41188756410644,1.41730276084749,
1.43084058397849,1.45101472565709,1.49357630988404,1.51136965632633,1.51559250277158,
1.51800787610396,1.52016188469643,1.52312080974288,1.5301823492393,1.54050794057009,
1.57534931570515,1.61237651259864,1.62165050138927,1.62639272592381,1.63018049920159,
1.63449363382543,1.64197198759118,1.68827555501049,1.72888793290298,1.73432736841164,
1.73703730628583,1.73921644847553,1.74151957718618,1.74523007548616,1.75831706971953,
1.78424581384169,1.83324275090273,1.84148685272035,1.84640241907379,1.85021948989542,
1.85438844787025,1.86119275138631,1.88833036670492,1.91645593292796,1.92484579996025,
1.95163644192558,1.95615739428983,1.95866430015579,1.96080002902903,1.96360332353323,
1.96976113670856,1.9974795461816,2.04742308357646,2.06052975701291,2.06602236058527,
2.06988229338644,2.07387199386493,2.07982730521795,2.09743024198081,2.12751039769845,
2.16992979139149,2.17582030821991,2.17857371361266,2.18070399666525,2.18324296864977,
2.18805348663228,2.19427456685343,2.20908608355818,2.2374776975812,2.27704904795642,
2.2843724340021,2.28869178348119,2.29243957129668,2.29714655932481,2.30656346429877,
2.31888721665889,2.35133919106459,2.39005584916645,2.39615404619614,2.39891498336828,
2.40104980462189,2.40355070418799,2.40817287159305,2.44279419766279,2.49508899561064,
2.5030484745972,2.50793628306202,2.51174021856224,2.51596804476606,2.52304226080094,
2.55492153642243,2.59780879562011,2.6137871040324,2.61788971530304,2.62028035171697,
2.62244948790057,2.62547794183238,2.63293492193362,2.64405309222125,2.66962673554813,
2.70117621828321,2.71983292544932,2.72609634153291,2.73015451659309,2.73402583299897,
2.73784961158552,2.74298847368029,2.75426624309546,2.77524983164141),
 .UNSPECIFIED.);
#1449=B_SPLINE_CURVE_WITH_KNOTS('',3,(#16189,#16190,#16191,#16192,#16193,
#16194,#16195,#16196,#16197,#16198,#16199,#16200,#16201,#16202,#16203,#16204,
#16205,#16206,#16207,#16208,#16209,#16210,#16211,#16212,#16213,#16214,#16215,
#16216,#16217,#16218,#16219,#16220,#16221,#16222,#16223,#16224,#16225,#16226,
#16227,#16228,#16229,#16230,#16231,#16232,#16233,#16234,#16235,#16236,#16237,
#16238,#16239,#16240,#16241,#16242,#16243,#16244,#16245,#16246,#16247,#16248,
#16249,#16250,#16251,#16252,#16253,#16254,#16255,#16256,#16257,#16258,#16259,
#16260,#16261,#16262,#16263,#16264,#16265,#16266,#16267,#16268,#16269,#16270,
#16271,#16272,#16273,#16274,#16275,#16276,#16277,#16278,#16279,#16280,#16281,
#16282,#16283,#16284,#16285,#16286,#16287,#16288,#16289,#16290,#16291,#16292,
#16293,#16294,#16295,#16296,#16297,#16298,#16299,#16300,#16301,#16302,#16303,
#16304,#16305,#16306,#16307,#16308,#16309,#16310,#16311,#16312,#16313,#16314,
#16315,#16316,#16317,#16318,#16319,#16320,#16321,#16322,#16323,#16324,#16325,
#16326,#16327,#16328,#16329,#16330,#16331,#16332,#16333,#16334,#16335,#16336,
#16337,#16338,#16339,#16340,#16341,#16342,#16343,#16344,#16345,#16346,#16347,
#16348,#16349,#16350,#16351,#16352,#16353,#16354,#16355,#16356,#16357,#16358,
#16359,#16360,#16361,#16362,#16363,#16364,#16365,#16366,#16367,#16368,#16369,
#16370,#16371,#16372,#16373,#16374,#16375,#16376,#16377,#16378,#16379,#16380,
#16381,#16382,#16383,#16384,#16385,#16386,#16387,#16388,#16389,#16390,#16391,
#16392,#16393,#16394,#16395,#16396,#16397,#16398),.UNSPECIFIED.,.F.,.F.,
(4,2,2,2,2,2,2,2,2,2,2,2,2,2,2,2,2,2,2,2,2,2,2,2,2,2,2,2,2,2,2,2,2,2,2,
2,2,2,2,2,2,2,2,2,2,2,2,2,2,2,2,2,2,2,2,2,2,2,2,2,2,2,2,2,2,2,2,2,2,2,2,
2,2,2,2,2,2,2,2,2,2,2,2,2,2,2,2,2,2,2,2,2,2,2,2,2,2,2,2,2,2,2,2,2,4),(0.000677522696600237,
0.0305089258241106,0.0357217105988039,0.0396135137556909,0.0435607528904782,
0.0477204696182164,0.0541915833973012,0.0741059967373185,0.115440097777174,
0.134317184493834,0.145106172757179,0.14864706152995,0.150963559598939,
0.153001420155386,0.155815446427006,0.163035034986156,0.217821138578187,
0.238208395197482,0.251873813278667,0.257357570144765,0.26129934021213,
0.26538551201792,0.271602298038433,0.289353198948155,0.339589261144455,
0.361984375015146,0.367591576073439,0.370311762371205,0.372252757395784,
0.374772116565687,0.379314809039923,0.406404733718979,0.414432682325065,
0.443038327387056,0.460786979930571,0.473151978164989,0.478396583079974,
0.482262594137674,0.486356375416247,0.492760354432907,0.51259909284976,
0.556547787118553,0.582188012129803,0.588138338702213,0.590907459740892,
0.592847503273448,0.595324546479347,0.599646787124584,0.619687590510394,
0.660066375923141,0.680065489411854,0.693550325746206,0.698995403707921,
0.702919464612365,0.706513885714489,0.711389222317492,0.723711801320998,
0.774193276476291,0.802031745603604,0.808230933663737,0.81106284263699,
0.813204901215941,0.815740344409894,0.820315956534282,0.848389345799933,
0.876342856806042,0.909948384155844,0.917146197055969,0.921427871307066,
0.9252687321384,0.930189007400477,0.938172509254794,0.999164983852803,1.01692011627422,
1.02727200361296,1.03071451736817,1.03297461344143,1.03498700860256,1.03776741267351,
1.04344525041317,1.07678153395365,1.10750510753919,1.13160484949986,1.1382267514405,
1.14238168193455,1.14625250349466,1.15133390112501,1.16295108822414,1.2146743273094,
1.24296511256131,1.24920253029659,1.25203487369017,1.25419112323307,1.2567231961712,
1.26128999367794,1.28892807428539,1.29537580787022,1.32175712996296,1.34142706453204,
1.35474982493395,1.36016555562901,1.36408011350876,1.36767367219295,1.37350241506738,
1.38838504316647),.UNSPECIFIED.);
#1450=B_SPLINE_CURVE_WITH_KNOTS('',3,(#16403,#16404,#16405,#16406,#16407,
#16408,#16409,#16410,#16411,#16412,#16413,#16414,#16415,#16416,#16417,#16418,
#16419,#16420,#16421,#16422,#16423,#16424,#16425,#16426,#16427,#16428,#16429,
#16430,#16431,#16432,#16433,#16434,#16435,#16436,#16437,#16438,#16439,#16440,
#16441,#16442,#16443,#16444,#16445,#16446,#16447,#16448,#16449,#16450,#16451,
#16452,#16453,#16454,#16455,#16456,#16457,#16458,#16459,#16460,#16461,#16462,
#16463,#16464,#16465,#16466,#16467,#16468,#16469,#16470,#16471,#16472,#16473,
#16474,#16475,#16476,#16477,#16478,#16479,#16480,#16481,#16482,#16483,#16484,
#16485,#16486,#16487,#16488,#16489,#16490,#16491,#16492,#16493,#16494,#16495,
#16496,#16497,#16498,#16499,#16500,#16501,#16502,#16503,#16504,#16505,#16506,
#16507,#16508,#16509,#16510,#16511,#16512,#16513,#16514,#16515,#16516,#16517,
#16518,#16519,#16520,#16521,#16522,#16523,#16524,#16525,#16526,#16527,#16528,
#16529,#16530,#16531,#16532,#16533,#16534,#16535,#16536,#16537,#16538,#16539,
#16540,#16541,#16542,#16543,#16544,#16545,#16546,#16547,#16548,#16549,#16550,
#16551,#16552,#16553,#16554,#16555,#16556,#16557,#16558,#16559,#16560,#16561,
#16562,#16563,#16564,#16565,#16566,#16567,#16568,#16569,#16570,#16571,#16572,
#16573,#16574,#16575,#16576,#16577,#16578,#16579,#16580,#16581,#16582,#16583,
#16584,#16585,#16586,#16587,#16588,#16589,#16590,#16591,#16592,#16593,#16594,
#16595,#16596,#16597,#16598),.UNSPECIFIED.,.F.,.F.,(4,2,2,2,2,2,2,2,2,2,
2,2,2,2,2,2,2,2,2,2,2,2,2,2,2,2,2,2,2,2,2,2,2,2,2,2,2,2,2,2,2,2,2,2,2,2,
2,2,2,2,2,2,2,2,2,2,2,2,2,2,2,2,2,2,2,2,2,2,2,2,2,2,2,2,2,2,2,2,2,2,2,2,
2,2,2,2,2,2,2,2,2,2,2,2,2,2,2,4),(0.00029246168118835,0.0328585636678094,
0.0667058328462643,0.0778435259812811,0.0828696078886542,0.0866900014310973,
0.0908461587794147,0.097592177913589,0.121093785472563,0.162881838567066,
0.180219822071848,0.190388972658726,0.193788250972792,0.196023740153427,
0.198017167485471,0.200771856106451,0.206396616707088,0.238925364174105,
0.266963907016703,0.294244321785116,0.301057788663898,0.305228435652312,
0.309044486884806,0.313955159749232,0.32218284537282,0.37135389164148,0.408175613816101,
0.412996223661644,0.415538634251756,0.417669540176693,0.420421537274337,
0.426304777495165,0.468914542634666,0.513239590782438,0.520844568367973,
0.525184629927034,0.528969383857968,0.533672976813764,0.542760084971374,
0.590969748200195,0.628864181011441,0.63355354838131,0.636068557916207,
0.638202427997394,0.640945550577899,0.646939191710579,0.687873371930506,
0.733784327768257,0.741346096652906,0.745676995844228,0.749462733365603,
0.75417927556698,0.763328775599775,0.810387242799095,0.837579976993194,
0.851030621355834,0.85477432184903,0.857084664002877,0.859259266550924,
0.861951867948976,0.868744858537939,0.912920490817548,0.940791392600704,
0.957582742793873,0.963439773532905,0.967408607838282,0.971282412503524,
0.976854716010281,0.990459250029259,1.03990459175393,1.06745386194676,1.0735937358375,
1.07639297618157,1.07852766872987,1.08103585188433,1.08556365529159,1.11268366089787,
1.11969753011607,1.1461997886862,1.16583340621934,1.17911405711989,1.18449016762945,
1.18836697719528,1.1919190330671,1.19766366486624,1.21233214987857,1.26072984825734,
1.28791979545175,1.29402325910311,1.29681596339525,1.29895021111714,1.30146329140139,
1.30601243315762,1.33451743269651,1.34130110590104,1.37019173079264,1.38769992508917,
1.38781753873472),.UNSPECIFIED.);
#1451=B_SPLINE_CURVE_WITH_KNOTS('',3,(#16599,#16600,#16601,#16602,#16603,
#16604,#16605,#16606,#16607,#16608,#16609,#16610,#16611,#16612,#16613,#16614,
#16615,#16616,#16617,#16618,#16619,#16620,#16621,#16622,#16623,#16624,#16625,
#16626,#16627,#16628,#16629,#16630,#16631,#16632,#16633,#16634,#16635,#16636,
#16637,#16638,#16639,#16640,#16641,#16642,#16643,#16644,#16645,#16646,#16647,
#16648,#16649,#16650,#16651,#16652,#16653,#16654,#16655,#16656,#16657,#16658,
#16659,#16660,#16661,#16662,#16663,#16664,#16665,#16666,#16667,#16668,#16669,
#16670,#16671,#16672,#16673,#16674,#16675,#16676,#16677,#16678,#16679,#16680,
#16681,#16682,#16683,#16684,#16685,#16686,#16687,#16688,#16689,#16690,#16691,
#16692,#16693,#16694,#16695,#16696,#16697,#16698,#16699,#16700,#16701,#16702,
#16703,#16704,#16705,#16706,#16707,#16708,#16709,#16710,#16711,#16712,#16713,
#16714,#16715,#16716,#16717,#16718,#16719,#16720,#16721,#16722,#16723,#16724,
#16725,#16726,#16727,#16728,#16729,#16730,#16731,#16732,#16733,#16734,#16735,
#16736,#16737,#16738,#16739,#16740,#16741,#16742,#16743,#16744,#16745,#16746,
#16747,#16748,#16749,#16750,#16751,#16752,#16753,#16754,#16755,#16756,#16757,
#16758,#16759,#16760,#16761,#16762,#16763,#16764,#16765,#16766,#16767,#16768,
#16769,#16770,#16771,#16772,#16773,#16774,#16775,#16776,#16777,#16778,#16779,
#16780,#16781,#16782,#16783,#16784,#16785,#16786,#16787,#16788,#16789,#16790,
#16791,#16792,#16793,#16794,#16795,#16796,#16797,#16798),.UNSPECIFIED.,
 .F.,.F.,(4,2,2,2,2,2,2,2,2,2,2,2,2,2,2,2,2,2,2,2,2,2,2,2,2,2,2,2,2,2,2,
2,2,2,2,2,2,2,2,2,2,2,2,2,2,2,2,2,2,2,2,2,2,2,2,2,2,2,2,2,2,2,2,2,2,2,2,
2,2,2,2,2,2,2,2,2,2,2,2,2,2,2,2,2,2,2,2,2,2,2,2,2,2,2,2,2,2,2,2,4),(1.38838504316647,
1.38850331657018,1.41256316811428,1.44667306241606,1.44811102723475,1.46649225057238,
1.47078026121916,1.47322547472784,1.47540162643616,1.4783881126609,1.48550725028072,
1.49592014500493,1.53121036702826,1.57078963891295,1.57821322467278,1.58258414872904,
1.58637316595498,1.59112839135375,1.60063468496618,1.61307917518895,1.64597237337316,
1.68389210018361,1.69005705102998,1.69284763421741,1.69500521915381,1.69753462282851,
1.70222009150174,1.70821798458257,1.75324208371746,1.79131622025913,1.79870369069099,
1.80306600069939,1.80685518199548,1.8116205870635,1.82118240752868,1.83372301547411,
1.86708290252621,1.90429856815899,1.91048908900112,1.91328403539824,1.9154419261792,
1.91796812267015,1.92263817328133,1.95937186695389,2.00891986627212,2.0171489199126,
2.02208526843446,2.02593676625895,2.03016270781747,2.03710709121351,2.06580112389977,
2.10529365796466,2.11401940909033,2.12837645384582,2.13235851468054,2.13473615847624,
2.13693609000036,2.14007345763307,2.14815486371714,2.16055820080493,2.2141235386633,
2.23416610497521,2.24061215811045,2.24473120291012,2.2486205794772,2.25389698809855,
2.26634447371481,2.28422675209128,2.31266795024048,2.32187714503914,2.34769990694516,
2.35222491717066,2.35474724607128,2.35688492438732,2.3597205397784,2.36597037686206,
2.39437673715468,2.44646960400029,2.45758228102903,2.46265717510102,2.46652855117249,
2.47068950817631,2.47733309926365,2.5016848784883,2.56327049652331,2.57095989607791,
2.57412270183141,2.57630528481707,2.57866621813506,2.58257291008395,2.59766209358923,
2.6311708372892,2.66962264116428,2.67899573405107,2.68378599503464,2.68761203478231,
2.6919694937766,2.69952942370826,2.74493413473101,2.77590460384327),
 .UNSPECIFIED.);
#1452=B_SPLINE_CURVE_WITH_KNOTS('',3,(#16804,#16805,#16806,#16807,#16808,
#16809,#16810,#16811,#16812,#16813,#16814,#16815,#16816,#16817,#16818,#16819,
#16820,#16821,#16822,#16823,#16824,#16825,#16826,#16827,#16828,#16829,#16830,
#16831,#16832,#16833,#16834,#16835,#16836,#16837,#16838,#16839,#16840,#16841,
#16842,#16843,#16844,#16845,#16846,#16847,#16848,#16849,#16850,#16851,#16852,
#16853,#16854,#16855,#16856,#16857,#16858,#16859,#16860,#16861,#16862,#16863,
#16864,#16865,#16866,#16867,#16868,#16869,#16870,#16871,#16872,#16873,#16874,
#16875,#16876,#16877,#16878,#16879,#16880,#16881,#16882,#16883,#16884,#16885,
#16886,#16887,#16888,#16889,#16890,#16891,#16892,#16893,#16894,#16895,#16896,
#16897,#16898,#16899,#16900,#16901,#16902,#16903,#16904,#16905,#16906,#16907,
#16908,#16909,#16910,#16911,#16912,#16913,#16914,#16915,#16916,#16917,#16918,
#16919,#16920,#16921,#16922,#16923,#16924,#16925,#16926,#16927,#16928,#16929,
#16930,#16931,#16932,#16933,#16934,#16935,#16936,#16937,#16938,#16939,#16940,
#16941,#16942,#16943,#16944,#16945,#16946,#16947,#16948,#16949,#16950,#16951,
#16952,#16953,#16954,#16955,#16956,#16957,#16958,#16959,#16960,#16961,#16962,
#16963,#16964,#16965,#16966,#16967,#16968,#16969,#16970,#16971,#16972,#16973,
#16974,#16975,#16976,#16977,#16978,#16979,#16980,#16981,#16982,#16983,#16984,
#16985,#16986,#16987,#16988,#16989,#16990,#16991,#16992,#16993,#16994,#16995,
#16996,#16997,#16998,#16999,#17000,#17001,#17002,#17003,#17004,#17005,#17006,
#17007,#17008,#17009,#17010,#17011,#17012,#17013),.UNSPECIFIED.,.F.,.F.,
(4,2,2,2,2,2,2,2,2,2,2,2,2,2,2,2,2,2,2,2,2,2,2,2,2,2,2,2,2,2,2,2,2,2,2,
2,2,2,2,2,2,2,2,2,2,2,2,2,2,2,2,2,2,2,2,2,2,2,2,2,2,2,2,2,2,2,2,2,2,2,2,
2,2,2,2,2,2,2,2,2,2,2,2,2,2,2,2,2,2,2,2,2,2,2,2,2,2,2,2,2,2,2,2,2,4),(1.38779141840252,
1.38798343212597,1.4200941295574,1.42466448576076,1.42718230209203,1.42931603129355,
1.43210214524226,1.43816902372091,1.46500213398631,1.51236265784808,1.52815980873776,
1.53406817122051,1.53765005781987,1.5415046631132,1.54675077690377,1.5592001045892,
1.57712914177577,1.60555853268652,1.61499139357061,1.64064669411246,1.64513951963695,
1.64764000456184,1.64975559015009,1.65255458380868,1.65869248426688,1.68622096081466,
1.73559073884686,1.74929574692861,1.75488677376961,1.75876424492972,1.76272908870636,
1.76856564521242,1.78519015610595,1.81261995164556,1.85542285589028,1.86363411170759,
1.86686333515655,1.86904240979612,1.87134558153992,1.87505658828857,1.88815045431959,
1.91410459456548,1.96304628452908,1.97129215603698,1.9762079341366,1.98002469242059,
1.98419282788319,1.99099467819026,2.01810242544466,2.04625021389738,2.05453441032295,
2.08143703927933,2.08595981212383,2.08846682702327,2.09060158029649,2.09340231752925,
2.09955071511475,2.12718617020335,2.17687348148206,2.19026267631174,2.19579648531033,
2.19966298905697,2.20364062338925,2.20954167656866,2.22669765154792,2.25554508800187,
2.29997330757964,2.30571580027897,2.30844114838567,2.31057019135909,2.31313303396502,
2.31805329943977,2.35104625300089,2.40466448394902,2.41247912984335,2.41732338293813,
2.42112060459359,2.42536903005419,2.4325461822975,2.46680266583386,2.49190339785816,
2.52223747407632,2.526779556272,2.52929069691744,2.53142462113234,2.53421861453376,
2.54033101365449,2.56761568812904,2.61628134863707,2.63068602467803,2.63638986867485,
2.63993416031327,2.6438163270291,2.6492257648443,2.66273138047077,2.68283935717001,
2.71721413585072,2.73655448432416,2.74511875093851,2.74840297010072,2.75039495632641,
2.7523847624689,2.75460988807712,2.75772530041555,2.77503528434477),
 .UNSPECIFIED.);
#1453=B_SPLINE_CURVE_WITH_KNOTS('',3,(#17014,#17015,#17016,#17017),
 .UNSPECIFIED.,.F.,.F.,(4,4),(0.000163392739190231,0.00029246168118835),
 .UNSPECIFIED.);
#1454=B_SPLINE_CURVE_WITH_KNOTS('',3,(#17019,#17020,#17021,#17022),
 .UNSPECIFIED.,.F.,.F.,(4,4),(2.77590460384327,2.77603086588106),
 .UNSPECIFIED.);
#1455=B_SPLINE_CURVE_WITH_KNOTS('',3,(#17023,#17024,#17025,#17026,#17027,
#17028,#17029,#17030,#17031,#17032,#17033,#17034,#17035,#17036,#17037,#17038,
#17039,#17040,#17041,#17042,#17043,#17044,#17045,#17046,#17047,#17048,#17049,
#17050,#17051,#17052,#17053,#17054,#17055,#17056,#17057,#17058,#17059,#17060,
#17061,#17062,#17063,#17064,#17065,#17066,#17067,#17068,#17069,#17070,#17071,
#17072,#17073,#17074,#17075,#17076,#17077,#17078,#17079,#17080,#17081,#17082,
#17083,#17084,#17085,#17086,#17087,#17088,#17089,#17090,#17091,#17092,#17093,
#17094,#17095,#17096,#17097,#17098,#17099,#17100,#17101,#17102,#17103,#17104,
#17105,#17106,#17107,#17108,#17109,#17110,#17111,#17112,#17113,#17114,#17115,
#17116,#17117,#17118,#17119,#17120,#17121,#17122,#17123,#17124,#17125,#17126,
#17127,#17128,#17129,#17130,#17131,#17132,#17133,#17134,#17135,#17136,#17137,
#17138,#17139,#17140,#17141,#17142,#17143,#17144,#17145,#17146,#17147,#17148,
#17149,#17150,#17151,#17152,#17153,#17154,#17155,#17156,#17157,#17158,#17159,
#17160,#17161,#17162,#17163,#17164,#17165,#17166,#17167,#17168,#17169,#17170,
#17171,#17172,#17173,#17174,#17175,#17176,#17177,#17178,#17179,#17180,#17181,
#17182,#17183,#17184,#17185,#17186,#17187,#17188,#17189,#17190,#17191,#17192,
#17193,#17194,#17195,#17196,#17197,#17198,#17199,#17200,#17201,#17202,#17203,
#17204,#17205,#17206,#17207,#17208,#17209,#17210,#17211,#17212,#17213,#17214,
#17215,#17216,#17217,#17218,#17219,#17220,#17221,#17222,#17223,#17224,#17225,
#17226,#17227,#17228,#17229,#17230,#17231,#17232),.UNSPECIFIED.,.F.,.F.,
(4,2,2,2,2,2,2,2,2,2,2,2,2,2,2,2,2,2,2,2,2,2,2,2,2,2,2,2,2,2,2,2,2,2,2,
2,2,2,2,2,2,2,2,2,2,2,2,2,2,2,2,2,2,2,2,2,2,2,2,2,2,2,2,2,2,2,2,2,2,2,2,
2,2,2,2,2,2,2,2,2,2,2,2,2,2,2,2,2,2,2,2,2,2,2,2,2,2,2,2,2,2,2,2,2,4),(0.000172071519088946,
0.00936200954417677,0.0149223775669653,0.017518380188118,0.0195753565284088,
0.0217251271889363,0.0244533148062466,0.0301257522401557,0.0487031491202788,
0.087748218640803,0.108099861116081,0.117389901349606,0.124970602857942,
0.129332630613796,0.133158342387564,0.137942465676234,0.14728499204543,
0.188635720076349,0.219885270247217,0.229668850919287,0.236467946344584,
0.239400183754385,0.241568242815474,0.244039959790243,0.248339588159849,
0.267928681029711,0.308718799179166,0.338827978987326,0.34585363499404,
0.350096838926966,0.353943539351612,0.358845602562056,0.366954519589289,
0.427304038829286,0.4515911703217,0.457408038422838,0.460163814382358,0.462108952690433,
0.464609661593327,0.469037341311807,0.491042611409219,0.529382799201337,
0.55931651300674,0.566332851140435,0.570574234803393,0.574421707536867,
0.579328066736765,0.589925139912958,0.64272496269062,0.671352346670467,
0.677624571272478,0.680464485685907,0.682602896576526,0.685123046349645,
0.68963732192096,0.715028593170323,0.724605226486315,0.752313070181977,
0.780010399846461,0.786893472118669,0.791106364215926,0.794961701941705,
0.799924852932101,0.808248318412805,0.856320024947246,0.894277998141745,
0.898976172261373,0.901508370041676,0.903665666865336,0.906452631902904,
0.912597330505417,0.950939765596203,0.983575954144689,1.00207891918968,
1.00817265736936,1.01221816215179,1.01610563912662,1.02159336246354,1.03439879193411,
1.08459299089626,1.11237275414485,1.11856079446773,1.12138557945048,1.12352262189201,
1.12605322828349,1.13061388620592,1.15792169624715,1.16475417716054,1.19125155847081,
1.2108201760337,1.22409352633608,1.22950078073953,1.23341301179958,1.2374905503967,
1.24373747271586,1.26194357533374,1.30706248408529,1.33542781675256,1.33997212116376,
1.34247181728779,1.34463451315869,1.34747062849104,1.35364978204733,1.38741841882821,
1.38761224885475),.UNSPECIFIED.);
#1456=B_SPLINE_CURVE_WITH_KNOTS('',3,(#17238,#17239,#17240,#17241),
 .UNSPECIFIED.,.F.,.F.,(4,4),(2.77512483966813,2.77514188312021),
 .UNSPECIFIED.);
#1457=B_SPLINE_CURVE_WITH_KNOTS('',3,(#17242,#17243,#17244,#17245,#17246,
#17247,#17248,#17249,#17250,#17251,#17252,#17253,#17254,#17255,#17256,#17257,
#17258,#17259,#17260,#17261,#17262,#17263,#17264,#17265,#17266,#17267,#17268,
#17269,#17270,#17271,#17272,#17273,#17274,#17275,#17276,#17277,#17278,#17279,
#17280,#17281,#17282,#17283,#17284,#17285,#17286,#17287,#17288,#17289,#17290,
#17291,#17292,#17293,#17294,#17295,#17296,#17297,#17298,#17299,#17300,#17301,
#17302,#17303,#17304,#17305,#17306,#17307,#17308,#17309,#17310,#17311,#17312,
#17313,#17314,#17315,#17316,#17317,#17318,#17319,#17320,#17321,#17322,#17323,
#17324,#17325,#17326,#17327,#17328,#17329,#17330,#17331,#17332,#17333,#17334,
#17335,#17336,#17337,#17338,#17339,#17340,#17341,#17342,#17343,#17344,#17345,
#17346,#17347,#17348,#17349,#17350,#17351,#17352,#17353,#17354,#17355,#17356,
#17357,#17358,#17359,#17360,#17361,#17362,#17363,#17364,#17365,#17366,#17367,
#17368,#17369,#17370,#17371,#17372,#17373,#17374,#17375,#17376,#17377,#17378,
#17379,#17380,#17381,#17382,#17383,#17384,#17385,#17386,#17387,#17388,#17389,
#17390,#17391,#17392,#17393,#17394,#17395,#17396,#17397,#17398,#17399,#17400,
#17401,#17402,#17403,#17404,#17405,#17406,#17407,#17408,#17409,#17410,#17411,
#17412,#17413,#17414,#17415,#17416,#17417,#17418,#17419,#17420,#17421,#17422,
#17423,#17424,#17425,#17426,#17427,#17428,#17429,#17430,#17431,#17432,#17433,
#17434,#17435,#17436,#17437,#17438,#17439,#17440,#17441),.UNSPECIFIED.,
 .F.,.F.,(4,2,2,2,2,2,2,2,2,2,2,2,2,2,2,2,2,2,2,2,2,2,2,2,2,2,2,2,2,2,2,
2,2,2,2,2,2,2,2,2,2,2,2,2,2,2,2,2,2,2,2,2,2,2,2,2,2,2,2,2,2,2,2,2,2,2,2,
2,2,2,2,2,2,2,2,2,2,2,2,2,2,2,2,2,2,2,2,2,2,2,2,2,2,2,2,2,2,2,2,4),(0.000192294988332048,
0.00607774719199029,0.0159169377236619,0.07398278467463,0.0901646279759542,
0.0967572037642757,0.101789524963687,0.104375587497259,0.10650371489967,
0.109202356866135,0.114803382211837,0.16059142721058,0.196384128692415,
0.207600242466767,0.212640225162752,0.216462826940986,0.220613265208185,
0.227331659049338,0.250360447559232,0.292397197982038,0.316101434412589,
0.321829231388031,0.324552020232788,0.326477015027514,0.328953908172427,
0.33334143309214,0.355071843920419,0.395089530730404,0.414212590606075,
0.42724804380981,0.432586554350752,0.436456819337085,0.44001704407753,0.445806861315989,
0.460777886563664,0.508888319781673,0.535978950451558,0.542072291622704,
0.544863168881321,0.546997240027056,0.549511512862563,0.554066242389265,
0.583546817453881,0.587892618058118,0.614224450006721,0.634122871496563,
0.643256189518113,0.650722921113714,0.655033860901014,0.658822355223786,
0.663569000615594,0.672863167770376,0.71546994844784,0.745873505836473,
0.755495636212241,0.762198933713271,0.765097778384368,0.767243682066841,
0.769690728384777,0.773946038582735,0.793176491308406,0.833021861268238,
0.864454730694058,0.871506455998565,0.875728489632487,0.879531940886113,
0.884425708407359,0.892408932896183,0.94443693775125,0.979190556805713,
0.983813268960183,0.986314367903372,0.988450298902266,0.991213530673869,
0.997317477465039,1.03601623075896,1.06850824923919,1.08084337654213,1.09026779983028,
1.09497866262644,1.09872966362081,1.10305293478694,1.11038375425721,1.14919005723998,
1.1774142228651,1.19277177394523,1.20214101896883,1.20543966566109,1.20765446748141,
1.20994392277896,1.21359190852609,1.224891134927,1.2651457388595,1.30479198503359,
1.31214463190117,1.31643114138381,1.32022284661305,1.32500655037598,1.33261294246727,
1.38779141840252),.UNSPECIFIED.);
#1458=B_SPLINE_CURVE_WITH_KNOTS('',3,(#17443,#17444,#17445,#17446,#17447,
#17448,#17449,#17450,#17451,#17452,#17453,#17454,#17455,#17456,#17457,#17458,
#17459,#17460,#17461,#17462,#17463,#17464,#17465,#17466,#17467,#17468,#17469,
#17470,#17471,#17472,#17473,#17474,#17475,#17476,#17477,#17478,#17479,#17480,
#17481,#17482,#17483,#17484,#17485,#17486,#17487,#17488,#17489,#17490,#17491,
#17492,#17493,#17494,#17495,#17496,#17497,#17498,#17499,#17500,#17501,#17502,
#17503,#17504,#17505,#17506,#17507,#17508,#17509,#17510,#17511,#17512,#17513,
#17514,#17515,#17516,#17517,#17518,#17519,#17520,#17521,#17522,#17523,#17524,
#17525,#17526,#17527,#17528,#17529,#17530,#17531,#17532,#17533,#17534,#17535,
#17536,#17537,#17538,#17539,#17540,#17541,#17542,#17543,#17544,#17545,#17546,
#17547,#17548,#17549,#17550,#17551,#17552,#17553,#17554,#17555,#17556,#17557,
#17558,#17559,#17560,#17561,#17562,#17563,#17564,#17565,#17566,#17567,#17568,
#17569,#17570,#17571,#17572,#17573,#17574,#17575,#17576,#17577,#17578,#17579,
#17580,#17581,#17582,#17583,#17584,#17585,#17586,#17587,#17588,#17589,#17590,
#17591,#17592,#17593,#17594,#17595,#17596,#17597,#17598,#17599,#17600,#17601,
#17602,#17603,#17604,#17605,#17606,#17607,#17608,#17609,#17610,#17611,#17612,
#17613,#17614,#17615,#17616,#17617,#17618,#17619,#17620,#17621,#17622,#17623,
#17624,#17625,#17626,#17627,#17628,#17629,#17630,#17631,#17632,#17633,#17634,
#17635,#17636,#17637,#17638,#17639,#17640),.UNSPECIFIED.,.F.,.F.,(4,2,2,
2,2,2,2,2,2,2,2,2,2,2,2,2,2,2,2,2,2,2,2,2,2,2,2,2,2,2,2,2,2,2,2,2,2,2,2,
2,2,2,2,2,2,2,2,2,2,2,2,2,2,2,2,2,2,2,2,2,2,2,2,2,2,2,2,2,2,2,2,2,2,2,2,
2,2,2,2,2,2,2,2,2,2,2,2,2,2,2,2,2,2,2,2,2,2,2,4),(1.38761224885475,1.4375036834497,
1.44569227850445,1.45061742311542,1.45446772566586,1.45870005310481,1.46567288350149,
1.49483724008579,1.53528308292903,1.55609614703464,1.56047418521489,1.56296387561242,
1.56491109692638,1.56768378278985,1.57358957035062,1.59867955919373,1.64123407087175,
1.66244243379664,1.66901419641069,1.67316053539395,1.67703909251926,1.68224443940608,
1.69425472675965,1.7413424817255,1.75085880380665,1.77630312287379,1.78081890893236,
1.78333954448885,1.78547810079993,1.7883179040798,1.79458860908678,1.82319783612459,
1.87591877396272,1.88555676656238,1.89040085508792,1.89398340270088,1.89790512472803,
1.90336650767092,1.91699752311241,1.93731941143245,1.98024552865551,1.99740812312745,
2.00161523245294,2.00404217779395,2.00622305592542,2.00924428024446,2.01657765486436,
2.02742099020821,2.06581876662872,2.10174465708663,2.10915591987101,2.11348218716905,
2.11693013752729,2.12158335290285,2.13057192847698,2.16304397066469,2.21490148709462,
2.22092467880892,2.22368963628375,2.22584498402527,2.22839318537159,2.23316739266884,
2.27080250147295,2.31913182360865,2.32744321612165,2.33240298851514,2.33625790394365,
2.34047255901488,2.34736365037911,2.37518965446231,2.40276282874832,2.41235029489264,
2.43768200497963,2.44219440404535,2.44471415568999,2.44685263659423,2.44969322094216,
2.45596905321813,2.48463334787844,2.53752115695101,2.54805836137235,2.55300695126462,
2.55684944912774,2.56111202791627,2.56822714023535,2.60006810498364,2.63864476614718,
2.65848492538306,2.6627967589665,2.66527131939438,2.66743883486286,2.67036632329412,
2.67713710462138,2.68686653808941,2.71778445042413,2.76083141921413,2.76892977369379,
2.77242616593864,2.7752680731555),.UNSPECIFIED.);
#1459=B_SPLINE_CURVE_WITH_KNOTS('',3,(#17641,#17642,#17643,#17644),
 .UNSPECIFIED.,.F.,.F.,(4,4),(0.000193089214357908,0.000209030494615362),
 .UNSPECIFIED.);
#1460=B_SPLINE_CURVE_WITH_KNOTS('',3,(#17649,#17650,#17651,#17652,#17653,
#17654,#17655,#17656,#17657,#17658,#17659,#17660,#17661,#17662,#17663,#17664,
#17665,#17666,#17667,#17668,#17669,#17670,#17671,#17672,#17673,#17674,#17675,
#17676,#17677,#17678,#17679,#17680,#17681,#17682,#17683,#17684,#17685,#17686,
#17687,#17688,#17689,#17690,#17691,#17692,#17693,#17694,#17695,#17696,#17697,
#17698,#17699,#17700,#17701,#17702,#17703,#17704,#17705,#17706,#17707,#17708,
#17709,#17710,#17711,#17712,#17713,#17714,#17715,#17716,#17717,#17718,#17719,
#17720,#17721,#17722,#17723,#17724,#17725,#17726,#17727,#17728,#17729,#17730,
#17731,#17732,#17733,#17734,#17735,#17736,#17737,#17738,#17739,#17740,#17741,
#17742,#17743,#17744,#17745,#17746,#17747,#17748,#17749,#17750,#17751,#17752,
#17753,#17754,#17755,#17756,#17757,#17758,#17759,#17760,#17761,#17762,#17763,
#17764,#17765,#17766,#17767,#17768,#17769,#17770,#17771,#17772,#17773,#17774,
#17775,#17776,#17777,#17778,#17779,#17780,#17781,#17782,#17783,#17784,#17785,
#17786,#17787,#17788,#17789,#17790,#17791,#17792,#17793,#17794,#17795,#17796,
#17797,#17798,#17799,#17800,#17801,#17802,#17803,#17804,#17805,#17806,#17807,
#17808,#17809,#17810,#17811,#17812,#17813,#17814,#17815,#17816,#17817,#17818,
#17819,#17820,#17821,#17822,#17823,#17824,#17825,#17826,#17827,#17828,#17829,
#17830,#17831,#17832,#17833,#17834,#17835,#17836,#17837,#17838,#17839,#17840,
#17841,#17842,#17843,#17844,#17845,#17846,#17847,#17848,#17849,#17850),
 .UNSPECIFIED.,.F.,.F.,(4,2,2,2,2,2,2,2,2,2,2,2,2,2,2,2,2,2,2,2,2,2,2,2,
2,2,2,2,2,2,2,2,2,2,2,2,2,2,2,2,2,2,2,2,2,2,2,2,2,2,2,2,2,2,2,2,2,2,2,2,
2,2,2,2,2,2,2,2,2,2,2,2,2,2,2,2,2,2,2,2,2,2,2,2,2,2,2,2,2,2,2,2,2,2,2,2,
2,2,2,2,4),(1.38767510941596,1.43112339601124,1.44039605580476,1.44513822465615,
1.44892626641656,1.45324005326402,1.4607204652113,1.46987448009624,1.4898415576597,
1.52903693125285,1.55018848634903,1.55455167320753,1.55702308145833,1.55894891956946,
1.56167959070667,1.56744907664187,1.59152382227246,1.63398317565435,1.6562623897388,
1.66294678284684,1.667089862421,1.670914744851,1.67597115047239,1.68728264468901,
1.72447587287317,1.76838266036149,1.77360945357837,1.77626714490509,1.77843300468403,
1.78075910335023,1.78457427656286,1.79884019787084,1.82906442645773,1.8719474956498,
1.88123774140026,1.88598344359576,1.88977168520334,1.89408287462065,1.90155145899932,
1.94809725340194,1.98843599942715,1.99449305198681,1.99724772480496,1.99938273452405,
2.00188958904393,2.00653998509891,2.04160575405013,2.09322857418171,2.10125434864285,
2.1061077163419,2.10991600606091,2.11411582525755,2.12106500774562,2.15057975615587,
2.17704738011528,2.18456687635986,2.21123387371285,2.21575145986064,2.2182573269305,
2.22039224892657,2.22319470419431,2.22935251871928,2.25708114858392,2.30704362751151,
2.320151926046,2.32564359127026,2.32950235273933,2.33349037636555,2.33944222748397,
2.35702651517694,2.38705959140961,2.42953922260409,2.43542611973755,2.43817862954996,
2.44030938448975,2.44285093341491,2.44766816192961,2.48368691196931,2.53383013242079,
2.54198250244127,2.54687154157531,2.55068421411694,2.554864798135,2.56172602988879,
2.58976962046305,2.61718293651675,2.62711231982529,2.65212325591286,2.65659795418927,
2.65909406831023,2.66120976551139,2.66401387584751,2.67018195298076,2.69801670035432,
2.72985904665648,2.74368990936215,2.75988741174204,2.76571496966692,2.76972187890552,
2.77245863450725,2.77512483966813),.UNSPECIFIED.);
#1461=B_SPLINE_CURVE_WITH_KNOTS('',3,(#17851,#17852,#17853,#17854,#17855,
#17856,#17857,#17858,#17859,#17860,#17861,#17862,#17863,#17864,#17865,#17866,
#17867,#17868,#17869,#17870,#17871,#17872,#17873,#17874,#17875,#17876,#17877,
#17878,#17879,#17880,#17881,#17882,#17883,#17884,#17885,#17886,#17887,#17888,
#17889,#17890,#17891,#17892,#17893,#17894,#17895,#17896,#17897,#17898,#17899,
#17900,#17901,#17902,#17903,#17904,#17905,#17906,#17907,#17908,#17909,#17910,
#17911,#17912,#17913,#17914,#17915,#17916,#17917,#17918,#17919,#17920,#17921,
#17922,#17923,#17924,#17925,#17926,#17927,#17928,#17929,#17930,#17931,#17932,
#17933,#17934,#17935,#17936,#17937,#17938,#17939,#17940,#17941,#17942,#17943,
#17944,#17945,#17946,#17947,#17948,#17949,#17950,#17951,#17952,#17953,#17954,
#17955,#17956,#17957,#17958,#17959,#17960,#17961,#17962,#17963,#17964,#17965,
#17966,#17967,#17968,#17969,#17970,#17971,#17972,#17973,#17974,#17975,#17976,
#17977,#17978,#17979,#17980,#17981,#17982,#17983,#17984,#17985,#17986,#17987,
#17988,#17989,#17990,#17991,#17992,#17993,#17994,#17995,#17996,#17997,#17998,
#17999,#18000,#18001,#18002,#18003,#18004,#18005,#18006,#18007,#18008,#18009,
#18010,#18011,#18012,#18013,#18014,#18015,#18016,#18017,#18018,#18019,#18020,
#18021,#18022,#18023,#18024,#18025,#18026,#18027,#18028,#18029,#18030,#18031,
#18032,#18033,#18034,#18035,#18036,#18037,#18038,#18039,#18040,#18041,#18042,
#18043,#18044,#18045,#18046,#18047,#18048),.UNSPECIFIED.,.F.,.F.,(4,2,2,
2,2,2,2,2,2,2,2,2,2,2,2,2,2,2,2,2,2,2,2,2,2,2,2,2,2,2,2,2,2,2,2,2,2,2,2,
2,2,2,2,2,2,2,2,2,2,2,2,2,2,2,2,2,2,2,2,2,2,2,2,2,2,2,2,2,2,2,2,2,2,2,2,
2,2,2,2,2,2,2,2,2,2,2,2,2,2,2,2,2,2,2,2,2,2,2,4),(0.000209030494615362,
0.00359170171313374,0.00801319147981052,0.0168020728302088,0.0773841769243228,
0.0952639350494035,0.105662925707357,0.109110945700868,0.111372170731263,
0.113384935493905,0.116163707070484,0.121830924692454,0.154946762097185,
0.185063790401504,0.209892269349023,0.216574301011722,0.220744210447303,
0.224613714204544,0.229671442592147,0.24113488885533,0.29299636669776,0.321327317194173,
0.32757058501874,0.330405434572305,0.332562866576736,0.335095005299073,
0.339662368457123,0.367341553470571,0.373741392744492,0.400169432933991,
0.429737036675418,0.436733589690745,0.440971115406994,0.444820258480975,
0.449735833184954,0.460382030936677,0.513136618016726,0.541751483294464,
0.54802297013801,0.550862995213566,0.553001681614494,0.555522386873839,
0.56003817770707,0.585465026779176,0.594666611669455,0.622067891505925,
0.650352030154785,0.657272765501373,0.661494139070315,0.66534780527941,
0.670295699394434,0.67856378793407,0.727558021069206,0.76440175930056,0.769282192585346,
0.771852685231552,0.774005962863598,0.776788042303393,0.78274306530777,
0.824305005342297,0.869604671686738,0.877203700112034,0.88157022621598,
0.885396356731324,0.890176359323216,0.899495816355134,0.942479013417658,
0.972514384964752,0.982094422924452,0.988788646646961,0.991703277619357,
0.993869516415409,0.996352090173414,1.00069820616056,1.02123427420754,1.06109214394567,
1.09113136745582,1.09815440120173,1.10239766390826,1.10624546199257,1.11115035099432,
1.1217365090302,1.17455898542707,1.20319545612348,1.20946913297048,1.21230958461967,
1.21444834878919,1.2169688539126,1.22148362417786,1.24687030071953,1.25645414820602,
1.28415538801843,1.31187016647005,1.31875518533815,1.32296893908029,1.32682485082551,
1.3317884416477,1.34011196177077,1.38801450560634),.UNSPECIFIED.);
#1462=B_SPLINE_CURVE_WITH_KNOTS('',3,(#18054,#18055,#18056,#18057),
 .UNSPECIFIED.,.F.,.F.,(4,4),(2.7753563039814,2.77545271603152),
 .UNSPECIFIED.);
#1463=B_SPLINE_CURVE_WITH_KNOTS('',3,(#18058,#18059,#18060,#18061,#18062,
#18063,#18064,#18065,#18066,#18067,#18068,#18069,#18070,#18071,#18072,#18073,
#18074,#18075,#18076,#18077,#18078,#18079,#18080,#18081,#18082,#18083,#18084,
#18085,#18086,#18087,#18088,#18089,#18090,#18091,#18092,#18093,#18094,#18095,
#18096,#18097,#18098,#18099,#18100,#18101,#18102,#18103,#18104,#18105,#18106,
#18107,#18108,#18109,#18110,#18111,#18112,#18113,#18114,#18115,#18116,#18117,
#18118,#18119,#18120,#18121,#18122,#18123,#18124,#18125,#18126,#18127,#18128,
#18129,#18130,#18131,#18132,#18133,#18134,#18135,#18136,#18137,#18138,#18139,
#18140,#18141,#18142,#18143,#18144,#18145,#18146,#18147,#18148,#18149,#18150,
#18151,#18152,#18153,#18154,#18155,#18156,#18157,#18158,#18159,#18160,#18161,
#18162,#18163,#18164,#18165,#18166,#18167,#18168,#18169,#18170,#18171,#18172,
#18173,#18174,#18175,#18176,#18177,#18178,#18179,#18180,#18181,#18182,#18183,
#18184,#18185,#18186,#18187,#18188,#18189,#18190,#18191,#18192,#18193,#18194,
#18195,#18196,#18197,#18198,#18199,#18200,#18201,#18202,#18203,#18204,#18205,
#18206,#18207,#18208,#18209,#18210,#18211,#18212,#18213,#18214,#18215,#18216,
#18217,#18218,#18219,#18220,#18221,#18222,#18223,#18224,#18225,#18226,#18227,
#18228,#18229,#18230,#18231,#18232,#18233,#18234,#18235,#18236,#18237,#18238,
#18239,#18240,#18241,#18242,#18243,#18244,#18245,#18246,#18247,#18248,#18249,
#18250,#18251,#18252,#18253,#18254,#18255,#18256,#18257),.UNSPECIFIED.,
 .F.,.F.,(4,2,2,2,2,2,2,2,2,2,2,2,2,2,2,2,2,2,2,2,2,2,2,2,2,2,2,2,2,2,2,
2,2,2,2,2,2,2,2,2,2,2,2,2,2,2,2,2,2,2,2,2,2,2,2,2,2,2,2,2,2,2,2,2,2,2,2,
2,2,2,2,2,2,2,2,2,2,2,2,2,2,2,2,2,2,2,2,2,2,2,2,2,2,2,2,2,2,2,2,4),(0.000182437931283686,
0.00653692196294665,0.0108609769573606,0.0130104903736253,0.0150542688106974,
0.0174265179469178,0.0214524366139877,0.0365305767037021,0.0787787328981987,
0.112285268459346,0.119432154772533,0.123674304161217,0.127473076906101,
0.132329194520251,0.140183791302266,0.193418740748948,0.227209744564475,
0.231821371483504,0.234319960305755,0.236455980335452,0.239222140074427,
0.245343379061742,0.283777908787235,0.316431851796508,0.328800611429692,
0.338244415141556,0.342958716191094,0.346709629394816,0.351029672091661,
0.358347407511598,0.399293664646039,0.432218473687358,0.443319513919408,
0.450765804092565,0.453786996395798,0.455950525789809,0.458336648643501,
0.462425926225514,0.478257660101814,0.51518183976668,0.552858135690341,
0.560156493659421,0.564431148432792,0.568224274037932,0.573025854561165,
0.580693819723936,0.63554907648934,0.66809932039209,0.672694513102882,0.675189667523938,
0.677326268798803,0.680097618843394,0.686023781836444,0.726898002540094,
0.772857763492995,0.780420281881811,0.7847513199462,0.788537009749807,0.793253270518437,
0.802401512598282,0.849485432533971,0.888475380488218,0.893122875235794,
0.895629066872899,0.897764063953238,0.90051945331205,0.90658077126419,0.946906838339564,
0.978290226453303,0.99634421909439,1.00235065791773,1.0063501174987,1.01020134143816,
1.01565028997868,1.0284328994166,1.07868462375402,1.10650661952783,1.11267410875596,
1.11547842035182,1.11759449172151,1.12009127611521,1.12456776472346,1.14960733215508,
1.15925455897892,1.18662796642128,1.21498656698914,1.22186840447295,1.2260539053021,
1.22986613635138,1.23474780735677,1.24287251263121,1.29338128185761,1.32937531542901,
1.33400890093295,1.33651227482695,1.33864784944877,1.3414077292625,1.34749320595248,
1.38747360616315,1.38767510941596),.UNSPECIFIED.);
#1464=B_SPLINE_CURVE_WITH_KNOTS('',3,(#18259,#18260,#18261,#18262,#18263,
#18264,#18265,#18266,#18267,#18268,#18269,#18270,#18271,#18272,#18273,#18274,
#18275,#18276,#18277,#18278,#18279,#18280,#18281,#18282,#18283,#18284,#18285,
#18286,#18287,#18288,#18289,#18290,#18291,#18292,#18293,#18294,#18295,#18296,
#18297,#18298,#18299,#18300,#18301,#18302,#18303,#18304,#18305,#18306,#18307,
#18308,#18309,#18310,#18311,#18312,#18313,#18314,#18315,#18316,#18317,#18318,
#18319,#18320,#18321,#18322,#18323,#18324,#18325,#18326,#18327,#18328,#18329,
#18330,#18331,#18332,#18333,#18334,#18335,#18336,#18337,#18338,#18339,#18340,
#18341,#18342,#18343,#18344,#18345,#18346,#18347,#18348,#18349,#18350,#18351,
#18352,#18353,#18354,#18355,#18356,#18357,#18358,#18359,#18360,#18361,#18362,
#18363,#18364,#18365,#18366,#18367,#18368,#18369,#18370,#18371,#18372,#18373,
#18374,#18375,#18376,#18377,#18378,#18379,#18380,#18381,#18382,#18383,#18384,
#18385,#18386,#18387,#18388,#18389,#18390,#18391,#18392,#18393,#18394,#18395,
#18396,#18397,#18398,#18399,#18400,#18401,#18402,#18403,#18404,#18405,#18406,
#18407,#18408,#18409,#18410,#18411,#18412,#18413,#18414,#18415,#18416,#18417,
#18418,#18419,#18420,#18421,#18422,#18423,#18424,#18425,#18426,#18427,#18428,
#18429,#18430,#18431,#18432,#18433,#18434,#18435,#18436,#18437,#18438,#18439,
#18440,#18441,#18442,#18443,#18444,#18445,#18446,#18447,#18448,#18449,#18450,
#18451,#18452,#18453,#18454,#18455,#18456,#18457,#18458,#18459,#18460,#18461,
#18462),.UNSPECIFIED.,.F.,.F.,(4,2,2,2,2,2,2,2,2,2,2,2,2,2,2,2,2,2,2,2,
2,2,2,2,2,2,2,2,2,2,2,2,2,2,2,2,2,2,2,2,2,2,2,2,2,2,2,2,2,2,2,2,2,2,2,2,
2,2,2,2,2,2,2,2,2,2,2,2,2,2,2,2,2,2,2,2,2,2,2,2,2,2,2,2,2,2,2,2,2,2,2,2,
2,2,2,2,2,2,2,2,2,4),(1.38801450560634,1.38821456747388,1.42369817782745,
1.42987238324046,1.43270770026876,1.4348704745835,1.43737103384921,1.44191880317453,
1.47039613150064,1.51578708719391,1.53371666506104,1.53993350385607,1.54400493083112,
1.54792120899495,1.55335026593637,1.56676498054793,1.58662744885994,1.6245372297973,
1.64695043283158,1.65139870467833,1.65390430628611,1.65584906348525,1.65859891302686,
1.6643829672707,1.68837409257627,1.74936329691702,1.7573420296936,1.76225984412887,
1.7660990874891,1.77037923682112,1.77757505223168,1.81117244864818,1.83932650150939,
1.86722547611572,1.87179560628477,1.87432829162228,1.87648550929775,1.87931922885402,
1.88555670049086,1.91383161529013,1.96551092154086,1.9770161386787,1.98170015466075,
1.98559929567117,1.98962758954039,1.99563829100745,2.01341542365613,2.04391184079909,
2.08555536014992,2.09150136733144,2.0942814291946,2.09643418581836,2.09900527847287,
2.10389012439133,2.14162809669519,2.18962680149004,2.19795596139163,2.20292051357819,
2.20677582364425,2.21098756183324,2.21786618783751,2.24550421666454,2.27323503645635,
2.28273971127688,2.30819372340121,2.31270911565288,2.31522940366754,2.31736757956771,
2.32020676598859,2.32647567800876,2.35507271951081,2.40776159121395,2.41847558330981,
2.42340255888651,2.42725248056222,2.43148253927356,2.43844730970399,2.46749164939931,
2.50853866858637,2.52893119103873,2.5332724157782,2.53575350135751,2.53791934118645,
2.54083469188214,2.54753569624607,2.55713056954624,2.58725526451146,2.63013596140322,
2.63945693115457,2.64423649514728,2.64806167924772,2.65242647931279,2.66002084554227,
2.70519835219979,2.73064921276551,2.74894487887096,2.75350970097938,2.75604098286511,
2.75817777618934,2.76029487092824,2.76308355449852,2.77549281338982),
 .UNSPECIFIED.);
#1465=B_SPLINE_CURVE_WITH_KNOTS('',3,(#18463,#18464,#18465,#18466),
 .UNSPECIFIED.,.F.,.F.,(4,4),(0.000175379134418719,0.000274764919486373),
 .UNSPECIFIED.);
#1466=B_SPLINE_CURVE_WITH_KNOTS('',3,(#18471,#18472,#18473,#18474,#18475,
#18476,#18477,#18478,#18479,#18480,#18481,#18482,#18483,#18484,#18485,#18486,
#18487,#18488,#18489,#18490,#18491,#18492,#18493,#18494,#18495,#18496,#18497,
#18498,#18499,#18500,#18501,#18502,#18503,#18504,#18505,#18506,#18507,#18508,
#18509,#18510,#18511,#18512,#18513,#18514,#18515,#18516,#18517,#18518,#18519,
#18520,#18521,#18522,#18523,#18524,#18525,#18526,#18527,#18528,#18529,#18530,
#18531,#18532,#18533,#18534,#18535,#18536,#18537,#18538,#18539,#18540,#18541,
#18542,#18543,#18544,#18545,#18546,#18547,#18548,#18549,#18550,#18551,#18552,
#18553,#18554,#18555,#18556,#18557,#18558,#18559,#18560,#18561,#18562,#18563,
#18564,#18565,#18566,#18567,#18568,#18569,#18570,#18571,#18572,#18573,#18574,
#18575,#18576,#18577,#18578,#18579,#18580,#18581,#18582,#18583,#18584,#18585,
#18586,#18587,#18588,#18589,#18590,#18591,#18592,#18593,#18594,#18595,#18596,
#18597,#18598,#18599,#18600,#18601,#18602,#18603,#18604,#18605,#18606,#18607,
#18608,#18609,#18610,#18611,#18612,#18613,#18614,#18615,#18616,#18617,#18618,
#18619,#18620,#18621,#18622,#18623,#18624,#18625,#18626,#18627,#18628,#18629,
#18630,#18631,#18632,#18633,#18634,#18635,#18636,#18637,#18638,#18639,#18640,
#18641,#18642,#18643,#18644,#18645,#18646,#18647,#18648,#18649,#18650,#18651,
#18652,#18653,#18654,#18655,#18656,#18657,#18658,#18659,#18660,#18661,#18662,
#18663,#18664,#18665,#18666,#18667,#18668,#18669,#18670),.UNSPECIFIED.,
 .F.,.F.,(4,2,2,2,2,2,2,2,2,2,2,2,2,2,2,2,2,2,2,2,2,2,2,2,2,2,2,2,2,2,2,
2,2,2,2,2,2,2,2,2,2,2,2,2,2,2,2,2,2,2,2,2,2,2,2,2,2,2,2,2,2,2,2,2,2,2,2,
2,2,2,2,2,2,2,2,2,2,2,2,2,2,2,2,2,2,2,2,2,2,2,2,2,2,2,2,2,2,2,2,4),(1.38783032955465,
1.38797382247406,1.42164717525487,1.45687548489826,1.46249483302315,1.46524838667397,
1.46724168212058,1.46947786297659,1.47287966671787,1.48306736885704,1.50045347420167,
1.54234804406643,1.56573909297665,1.57247812833265,1.57663306124756,1.58045434953077,
1.5854845802705,1.5966444173606,1.63111992479794,1.67316555063445,1.68224445455045,
1.68560198432229,1.6876079490253,1.68982914228136,1.69315900789914,1.7027688470521,
1.71870904191044,1.76597962238645,1.78669875942825,1.79317890893748,1.79727833693069,
1.80111968176933,1.8062841723444,1.81823369476285,1.8649872473264,1.87017244894104,
1.90031845774389,1.90487452889868,1.9073891600646,1.90952326180928,1.91231385939691,
1.91840532083447,1.94547724524786,1.99352125702125,2.00859085316158,2.01439529014585,
2.01795822203195,2.02182651726854,2.02715332607901,2.04011314850359,2.05907796824362,
2.08624978775251,2.09576383231955,2.12087042173293,2.12534848166642,2.12784564971207,
2.1299616925156,2.13276554675666,2.13893033033105,2.16672552088088,2.21688296002443,
2.22979164382826,2.23525711926235,2.23911134411923,2.24310649636951,2.24909197912153,
2.26696342902514,2.29781391881057,2.33900777215224,2.34497063530561,2.34770808693128,
2.34984141131703,2.35236043309928,2.35706911434152,2.3631197473591,2.37731632436639,
2.4063006888814,2.44622670283569,2.45353628082957,2.45785452368577,2.46160569764634,
2.46632271232396,2.4757804549929,2.48817189177434,2.52093544841506,2.55917949482486,
2.56529664159717,2.56806204196975,2.57019797929527,2.57269703828066,2.5773109881588,
2.61125912562925,2.66433002274866,2.67220591481856,2.67706814950483,2.68086752354038,
2.68510602794984,2.69223625731738,2.72537166303582,2.7753563039814),
 .UNSPECIFIED.);
#1467=B_SPLINE_CURVE_WITH_KNOTS('',3,(#18671,#18672,#18673,#18674,#18675,
#18676,#18677,#18678,#18679,#18680,#18681,#18682,#18683,#18684,#18685,#18686,
#18687,#18688,#18689,#18690,#18691,#18692,#18693,#18694,#18695,#18696,#18697,
#18698,#18699,#18700,#18701,#18702,#18703,#18704,#18705,#18706,#18707,#18708,
#18709,#18710,#18711,#18712,#18713,#18714,#18715,#18716,#18717,#18718,#18719,
#18720,#18721,#18722,#18723,#18724,#18725,#18726,#18727,#18728,#18729,#18730,
#18731,#18732,#18733,#18734,#18735,#18736,#18737,#18738,#18739,#18740,#18741,
#18742,#18743,#18744,#18745,#18746,#18747,#18748,#18749,#18750,#18751,#18752,
#18753,#18754,#18755,#18756,#18757,#18758,#18759,#18760,#18761,#18762,#18763,
#18764,#18765,#18766,#18767,#18768,#18769,#18770,#18771,#18772,#18773,#18774,
#18775,#18776,#18777,#18778,#18779,#18780,#18781,#18782,#18783,#18784,#18785,
#18786,#18787,#18788,#18789,#18790,#18791,#18792,#18793,#18794,#18795,#18796,
#18797,#18798,#18799,#18800,#18801,#18802,#18803,#18804,#18805,#18806,#18807,
#18808,#18809,#18810,#18811,#18812,#18813,#18814,#18815,#18816,#18817,#18818,
#18819,#18820,#18821,#18822,#18823,#18824,#18825,#18826,#18827,#18828,#18829,
#18830,#18831,#18832,#18833,#18834,#18835,#18836,#18837,#18838,#18839,#18840,
#18841,#18842,#18843,#18844,#18845,#18846,#18847,#18848,#18849,#18850,#18851,
#18852,#18853,#18854,#18855,#18856,#18857,#18858,#18859,#18860,#18861,#18862,
#18863,#18864,#18865,#18866,#18867,#18868),.UNSPECIFIED.,.F.,.F.,(4,2,2,
2,2,2,2,2,2,2,2,2,2,2,2,2,2,2,2,2,2,2,2,2,2,2,2,2,2,2,2,2,2,2,2,2,2,2,2,
2,2,2,2,2,2,2,2,2,2,2,2,2,2,2,2,2,2,2,2,2,2,2,2,2,2,2,2,2,2,2,2,2,2,2,2,
2,2,2,2,2,2,2,2,2,2,2,2,2,2,2,2,2,2,2,2,2,2,2,4),(0.000274764919486373,
0.062895630461027,0.0813501395675178,0.0874374187852338,0.0914808653973023,
0.0953680021534591,0.100858040901126,0.113687483403507,0.163842339124501,
0.193602521989007,0.198516403059142,0.201093239299371,0.2032450839026,0.206016656515119,
0.211918773340013,0.254215798711661,0.267386429908165,0.288843042588712,
0.302995696994059,0.308533403799369,0.312468373296255,0.316035183053858,
0.320816070505866,0.332701264299013,0.383864897410737,0.411964006093194,
0.418183334875138,0.421013422479729,0.42315056372249,0.425676584954236,
0.430218191572825,0.456688328809736,0.464516978629412,0.465739291622078,
0.495293695956529,0.520819755702825,0.527553043852622,0.531733369714844,
0.535598121938227,0.540629010791724,0.551938814644686,0.603952953025513,
0.632329023987934,0.638576056771627,0.641411234767869,0.643568306936236,
0.646099303556593,0.650662943396744,0.678173056626024,0.684761543505955,
0.710982094544844,0.74070615673981,0.747710453462217,0.751949078120344,
0.755796928922688,0.760707714572317,0.768847256701182,0.819450935999529,
0.855260572573492,0.859923279949871,0.862447841705736,0.864605972203848,
0.867403266015435,0.873606362357614,0.910529596186081,0.944109446073919,
0.956695639037509,0.9662832342947,0.971053702999564,0.974843406677438,0.979202462142167,
0.986575095102644,1.02538752318016,1.0537871748655,1.0689472681226,1.07528063488783,
1.0801682480595,1.0827398339018,1.08489240967791,1.08767150247474,1.09361278042131,
1.13536556076732,1.18047633506502,1.18807044408786,1.19243522838387,1.19626046527789,
1.20104018437499,1.21036178088627,1.25312035944959,1.2833067121169,1.29758815417143,
1.30142838602475,1.30377475737461,1.30596503157037,1.30917005368632,1.31712542592157,
1.36014291061841,1.38762556260924,1.38776860835863),.UNSPECIFIED.);
#1468=B_SPLINE_CURVE_WITH_KNOTS('',3,(#18873,#18874,#18875,#18876,#18877,
#18878,#18879,#18880,#18881,#18882,#18883,#18884,#18885,#18886,#18887,#18888,
#18889,#18890,#18891,#18892,#18893,#18894,#18895,#18896,#18897,#18898,#18899,
#18900,#18901,#18902,#18903,#18904,#18905,#18906,#18907,#18908,#18909,#18910,
#18911,#18912,#18913,#18914,#18915,#18916,#18917,#18918,#18919,#18920,#18921,
#18922,#18923,#18924,#18925,#18926,#18927,#18928,#18929,#18930,#18931,#18932,
#18933,#18934,#18935,#18936,#18937,#18938,#18939,#18940,#18941,#18942,#18943,
#18944,#18945,#18946,#18947,#18948,#18949,#18950,#18951,#18952,#18953,#18954,
#18955,#18956,#18957,#18958,#18959,#18960,#18961,#18962,#18963,#18964,#18965,
#18966,#18967,#18968,#18969,#18970,#18971,#18972,#18973,#18974,#18975,#18976,
#18977,#18978,#18979,#18980,#18981,#18982,#18983,#18984,#18985,#18986,#18987,
#18988,#18989,#18990,#18991,#18992,#18993,#18994,#18995,#18996,#18997,#18998,
#18999,#19000,#19001,#19002,#19003,#19004,#19005,#19006,#19007,#19008,#19009,
#19010,#19011,#19012,#19013,#19014,#19015,#19016,#19017,#19018,#19019,#19020,
#19021,#19022,#19023,#19024,#19025,#19026,#19027,#19028,#19029,#19030,#19031,
#19032,#19033,#19034,#19035,#19036,#19037,#19038,#19039,#19040,#19041,#19042,
#19043,#19044,#19045,#19046,#19047,#19048,#19049,#19050,#19051,#19052,#19053,
#19054,#19055,#19056,#19057,#19058,#19059,#19060,#19061,#19062,#19063,#19064,
#19065,#19066,#19067,#19068,#19069,#19070,#19071,#19072,#19073,#19074,#19075,
#19076,#19077,#19078,#19079,#19080,#19081,#19082),.UNSPECIFIED.,.F.,.F.,
(4,2,2,2,2,2,2,2,2,2,2,2,2,2,2,2,2,2,2,2,2,2,2,2,2,2,2,2,2,2,2,2,2,2,2,
2,2,2,2,2,2,2,2,2,2,2,2,2,2,2,2,2,2,2,2,2,2,2,2,2,2,2,2,2,2,2,2,2,2,2,2,
2,2,2,2,2,2,2,2,2,2,2,2,2,2,2,2,2,2,2,2,2,2,2,2,2,2,2,2,2,2,2,2,2,4),(0.000324143214619982,
0.0158771094677429,0.0253256916034115,0.0295631149526927,0.0331209995144121,
0.0369092809154866,0.0416550921416168,0.0509457788737595,0.0784877923858483,
0.106581253516791,0.134349941563318,0.140511989900533,0.143315274440515,
0.145431199113102,0.147928564149414,0.152407811664709,0.17755282354848,
0.187425837957977,0.215085789515885,0.242886023539641,0.249733061851928,
0.253911016914234,0.257725176551781,0.262621503787905,0.270798138512466,
0.320633374637595,0.357196980464997,0.361834460025077,0.364338615408408,
0.366474015537369,0.369232612490268,0.375311223949213,0.41543612103427,
0.446945705212345,0.465043005415902,0.471054562112113,0.475055214859167,
0.478905955056057,0.484351423021017,0.497106441653766,0.54738762045425,
0.575220035847899,0.581388739115619,0.584193354432322,0.586328702210027,
0.588833595523762,0.593346086128498,0.6197635794788,0.628535276753099,0.656623833246853,
0.683846243736795,0.690656446574303,0.694826678539508,0.698643380678667,
0.70355632828705,0.711791100802504,0.760876544034798,0.786716483537455,
0.799777497874279,0.803485626225488,0.805788333016259,0.807968087090028,
0.810679787991711,0.816125831712701,0.856712147270895,0.903051367701181,
0.910541362758302,0.914857263670785,0.91864515240653,0.923384476776052,
0.932643004919074,0.976743445578183,1.00604596927801,1.0154782267772,1.02208292984193,
1.02496480091048,1.02710858112767,1.02956525578479,1.03386303786208,1.0533385937206,
1.09228763610114,1.11353353978246,1.12756660898495,1.133054960024,1.13695227586539,
1.1404826398124,1.14610351218811,1.15997305013599,1.20915166312345,1.23661077063823,
1.24274179985566,1.24553958605232,1.24767431703644,1.25018390355316,1.25471741155012,
1.28211555775354,1.28996158175801,1.31872987310898,1.3363563305562,1.34865284472729,
1.35387436658997,1.35772496048381,1.36180366957232,1.36818631869201,1.38783032955465),
 .UNSPECIFIED.);
#1469=B_SPLINE_CURVE_WITH_KNOTS('',3,(#19083,#19084,#19085,#19086,#19087,
#19088,#19089,#19090,#19091,#19092,#19093,#19094,#19095,#19096,#19097,#19098,
#19099,#19100,#19101,#19102,#19103,#19104,#19105,#19106,#19107,#19108,#19109,
#19110,#19111,#19112,#19113,#19114,#19115,#19116,#19117,#19118,#19119,#19120,
#19121,#19122,#19123,#19124,#19125,#19126,#19127,#19128,#19129,#19130,#19131,
#19132,#19133,#19134,#19135,#19136,#19137,#19138,#19139,#19140,#19141,#19142,
#19143,#19144,#19145,#19146,#19147,#19148,#19149,#19150,#19151,#19152,#19153,
#19154,#19155,#19156,#19157,#19158,#19159,#19160,#19161,#19162,#19163,#19164,
#19165,#19166,#19167,#19168,#19169,#19170,#19171,#19172,#19173,#19174,#19175,
#19176,#19177,#19178,#19179,#19180,#19181,#19182,#19183,#19184,#19185,#19186,
#19187,#19188,#19189,#19190,#19191,#19192,#19193,#19194,#19195,#19196,#19197,
#19198,#19199,#19200,#19201,#19202,#19203,#19204,#19205,#19206,#19207,#19208,
#19209,#19210,#19211,#19212,#19213,#19214,#19215,#19216,#19217,#19218,#19219,
#19220,#19221,#19222,#19223,#19224,#19225,#19226,#19227,#19228,#19229,#19230,
#19231,#19232,#19233,#19234,#19235,#19236,#19237,#19238,#19239,#19240,#19241,
#19242,#19243,#19244,#19245,#19246,#19247,#19248,#19249,#19250,#19251,#19252,
#19253,#19254,#19255,#19256,#19257,#19258,#19259,#19260,#19261,#19262,#19263,
#19264,#19265,#19266,#19267,#19268,#19269,#19270,#19271,#19272,#19273,#19274,
#19275,#19276,#19277,#19278,#19279,#19280,#19281,#19282,#19283,#19284,#19285,
#19286,#19287,#19288,#19289,#19290,#19291,#19292),.UNSPECIFIED.,.F.,.F.,
(4,2,2,2,2,2,2,2,2,2,2,2,2,2,2,2,2,2,2,2,2,2,2,2,2,2,2,2,2,2,2,2,2,2,2,
2,2,2,2,2,2,2,2,2,2,2,2,2,2,2,2,2,2,2,2,2,2,2,2,2,2,2,2,2,2,2,2,2,2,2,2,
2,2,2,2,2,2,2,2,2,2,2,2,2,2,2,2,2,2,2,2,2,2,2,2,2,2,2,2,2,2,2,2,2,4),(1.38776860835863,
1.40398233122755,1.41000183807035,1.41362896188388,1.41751622842159,1.42277942376607,
1.43514507724354,1.45286443649362,1.48147220501137,1.49001685060718,1.51658431760489,
1.52112803959449,1.52365458190256,1.52579170351979,1.52862120717566,1.53483702891505,
1.56290070147281,1.61394052191223,1.62593366204401,1.63074978837543,1.63432506904011,
1.63825192507432,1.6437451301814,1.65759438927064,1.67838678690219,1.71798829944731,
1.73743485000576,1.74172687122125,1.74419674243102,1.74636498010362,1.74929993172342,
1.75611578834237,1.7659331722403,1.79738558949043,1.83850355419817,1.84784905440877,
1.85263353141662,1.85645895418144,1.86082003317611,1.86839750174269,1.91347260255677,
1.95524989945497,1.96118744088172,1.96396570133679,1.96611807457362,1.96868992327123,
1.97357941726164,1.97991658792669,1.99509159111867,2.02349581203877,2.06231521828226,
2.06968847118898,2.07404744963738,2.0778368148891,2.08260649948585,2.09219132972863,
2.10477186058338,2.13832904620017,2.17523617074205,2.18143716845065,2.18423391208206,
2.18639181423807,2.18891630482129,2.19357942337749,2.22942487332542,2.28001356930114,
2.28815621832208,2.29306756991374,2.2969151245303,2.3011526657105,2.30815341316567,
2.33783121018183,2.36407119171349,2.37073182078227,2.3981507716049,2.40271189030694,
2.40524214474599,2.40739899658415,2.41023446382361,2.41648423979278,2.44489287544769,
2.49698879118486,2.50809140785172,2.51316420984523,2.51703500955063,2.52119634034231,
2.52784270954923,2.55223478687431,2.60654278757697,2.61989508290732,2.62378478291468,
2.62614182645868,2.62835137441456,2.63154348302303,2.63999967044271,2.65322071616338,
2.68708746236375,2.71557822445905,2.72780807222084,2.73266290825367,2.73624748959956,
2.74016571088565,2.74404832192756,2.7493056597695,2.77503853942652),
 .UNSPECIFIED.);
#1470=B_SPLINE_CURVE_WITH_KNOTS('',3,(#19298,#19299,#19300,#19301,#19302,
#19303,#19304,#19305,#19306,#19307,#19308,#19309,#19310,#19311,#19312,#19313,
#19314,#19315,#19316,#19317,#19318,#19319,#19320,#19321,#19322,#19323,#19324,
#19325,#19326,#19327,#19328,#19329,#19330,#19331,#19332,#19333,#19334,#19335,
#19336,#19337,#19338,#19339,#19340,#19341,#19342,#19343,#19344,#19345,#19346,
#19347,#19348,#19349,#19350,#19351,#19352,#19353,#19354,#19355,#19356,#19357,
#19358,#19359,#19360,#19361,#19362,#19363,#19364,#19365,#19366,#19367,#19368,
#19369,#19370,#19371,#19372,#19373,#19374,#19375,#19376,#19377,#19378,#19379,
#19380,#19381,#19382,#19383,#19384,#19385,#19386,#19387,#19388,#19389,#19390,
#19391,#19392,#19393,#19394,#19395,#19396,#19397,#19398,#19399,#19400,#19401,
#19402,#19403,#19404,#19405,#19406,#19407,#19408,#19409,#19410,#19411,#19412,
#19413,#19414,#19415,#19416,#19417,#19418,#19419,#19420,#19421,#19422,#19423,
#19424,#19425,#19426,#19427,#19428,#19429,#19430,#19431,#19432,#19433,#19434,
#19435,#19436,#19437,#19438,#19439,#19440,#19441,#19442,#19443,#19444,#19445,
#19446,#19447,#19448,#19449,#19450,#19451,#19452,#19453,#19454,#19455,#19456,
#19457,#19458,#19459,#19460,#19461,#19462,#19463,#19464,#19465,#19466,#19467,
#19468,#19469,#19470,#19471,#19472,#19473,#19474,#19475,#19476,#19477,#19478,
#19479,#19480,#19481,#19482,#19483,#19484,#19485,#19486,#19487,#19488,#19489,
#19490,#19491),.UNSPECIFIED.,.F.,.F.,(4,2,2,2,2,2,2,2,2,2,2,2,2,2,2,2,2,
2,2,2,2,2,2,2,2,2,2,2,2,2,2,2,2,2,2,2,2,2,2,2,2,2,2,2,2,2,2,2,2,2,2,2,2,
2,2,2,2,2,2,2,2,2,2,2,2,2,2,2,2,2,2,2,2,2,2,2,2,2,2,2,2,2,2,2,2,2,2,2,2,
2,2,2,2,2,2,2,4),(1.38751651967754,1.39697591777425,1.42674998314585,1.4702579200917,
1.47953589550948,1.48427962318721,1.48806835250533,1.49238232116074,1.49986148827734,
1.54615730070722,1.58679397815463,1.59223249451174,1.59494253514564,1.59712204235159,
1.59942583509039,1.60313813181305,1.61623976683816,1.64221612717862,1.6911439151196,
1.69939330148544,1.7043106590849,1.70812834945081,1.71229720636026,1.71909955459103,
1.74619760867662,1.77436384398711,1.78258875633297,1.80956214071788,1.81408731392465,
1.81659520388562,1.81873040026365,1.82153132476725,1.82767865010866,1.85529595906221,
1.90492261126032,1.91838594168092,1.92393318028493,1.9278028212278,1.931778455983,
1.93766657364923,1.95470800629132,1.9832413031419,2.02824017418,2.03392619157339,
2.03664117836699,2.03877012997708,2.04134256263214,2.04630781598199,2.08070180057313,
2.13251105184096,2.14052006760041,2.14542138815011,2.14922587314184,2.15344413127749,
2.16047776650624,2.19155381143962,2.23362429189789,2.25116751938539,2.25537199407536,
2.25778342871889,2.25993890114918,2.26290649436243,2.27001912405128,2.28044606894956,
2.31597917370023,2.35549686073998,2.36282374805078,2.36714617676002,2.37089733628049,
2.37560955867643,2.38504086394715,2.39738654447141,2.42993011092691,2.46850666193667,
2.47461557824794,2.47737968713199,2.47951570600553,2.48201615913376,2.48663588685027,
2.52105538985485,2.57357844702098,2.58149697303046,2.5863718984084,2.59017308388314,
2.59419656196975,2.60083417866563,2.6088647789538,2.62524974937419,2.6689731736202,
2.69156590513936,2.69599526701249,2.69848152159372,2.70040503240681,2.70311443853625,
2.70877221380305,2.73186702711985,2.77508623523689),.UNSPECIFIED.);
#1471=B_SPLINE_CURVE_WITH_KNOTS('',3,(#19492,#19493,#19494,#19495),
 .UNSPECIFIED.,.F.,.F.,(4,4),(0.00015374700249208,0.000324143214619982),
 .UNSPECIFIED.);
#1472=B_SPLINE_CURVE_WITH_KNOTS('',3,(#19497,#19498,#19499,#19500),
 .UNSPECIFIED.,.F.,.F.,(4,4),(2.77503853942652,2.77520897093981),
 .UNSPECIFIED.);
#1473=B_SPLINE_CURVE_WITH_KNOTS('',3,(#19501,#19502,#19503,#19504,#19505,
#19506,#19507,#19508,#19509,#19510,#19511,#19512,#19513,#19514,#19515,#19516,
#19517,#19518,#19519,#19520,#19521,#19522,#19523,#19524,#19525,#19526,#19527,
#19528,#19529,#19530,#19531,#19532,#19533,#19534,#19535,#19536,#19537,#19538,
#19539,#19540,#19541,#19542,#19543,#19544,#19545,#19546,#19547,#19548,#19549,
#19550,#19551,#19552,#19553,#19554,#19555,#19556,#19557,#19558,#19559,#19560,
#19561,#19562,#19563,#19564,#19565,#19566,#19567,#19568,#19569,#19570,#19571,
#19572,#19573,#19574,#19575,#19576,#19577,#19578,#19579,#19580,#19581,#19582,
#19583,#19584,#19585,#19586,#19587,#19588,#19589,#19590,#19591,#19592,#19593,
#19594,#19595,#19596,#19597,#19598,#19599,#19600,#19601,#19602,#19603,#19604,
#19605,#19606,#19607,#19608,#19609,#19610,#19611,#19612,#19613,#19614,#19615,
#19616,#19617,#19618,#19619,#19620,#19621,#19622,#19623,#19624,#19625,#19626,
#19627,#19628,#19629,#19630,#19631,#19632,#19633,#19634,#19635,#19636,#19637,
#19638,#19639,#19640,#19641,#19642,#19643,#19644,#19645,#19646,#19647,#19648,
#19649,#19650,#19651,#19652,#19653,#19654,#19655,#19656,#19657,#19658,#19659,
#19660,#19661,#19662,#19663,#19664,#19665,#19666,#19667,#19668,#19669,#19670,
#19671,#19672,#19673,#19674,#19675,#19676,#19677,#19678,#19679,#19680,#19681,
#19682,#19683,#19684,#19685,#19686,#19687,#19688,#19689,#19690,#19691,#19692,
#19693,#19694,#19695,#19696,#19697,#19698,#19699,#19700,#19701,#19702,#19703,
#19704,#19705,#19706,#19707,#19708,#19709,#19710,#19711,#19712,#19713,#19714,
#19715,#19716),.UNSPECIFIED.,.F.,.F.,(4,2,2,2,2,2,2,2,2,2,2,2,2,2,2,2,2,
2,2,2,2,2,2,2,2,2,2,2,2,2,2,2,2,2,2,2,2,2,2,2,2,2,2,2,2,2,2,2,2,2,2,2,2,
2,2,2,2,2,2,2,2,2,2,2,2,2,2,2,2,2,2,2,2,2,2,2,2,2,2,2,2,2,2,2,2,2,2,2,2,
2,2,2,2,2,2,2,2,2,2,2,2,2,2,2,2,2,2,4),(0.000144395392494094,0.0335360417482643,
0.061369564427443,0.0675626175607466,0.0703881121110802,0.0725444079601289,
0.0750822964663496,0.0796765049185713,0.111407318138572,0.146349092280614,
0.162357644088658,0.173765973228149,0.178382268974139,0.178526076332496,
0.178673879658054,0.178826415336729,0.178984514681895,0.179149125689295,
0.17932134022883,0.17938678786255,0.179473112109535,0.179588328256961,0.183377949240674,
0.187737567173298,0.195112746848084,0.23389246083911,0.262199201363727,
0.277437258647108,0.283791911916812,0.288692226521834,0.291266435908779,
0.293418773028459,0.296194430520708,0.302117353072285,0.344260863152019,
0.389019310541182,0.396607313634844,0.400970789500911,0.404796164070481,
0.409577747284325,0.418908453871539,0.461166385467933,0.491726531638866,
0.501394769547792,0.508134262805267,0.5110562327663,0.513222920003422,0.515700240096551,
0.520024840959891,0.540130580129801,0.578664439233278,0.610310550593883,
0.617415996861764,0.621676253185538,0.625518823943701,0.630470554248946,
0.641026657918823,0.693866049261419,0.722504761659807,0.72877777371306,
0.731617667780256,0.733755901598967,0.736275649268416,0.740788762352783,
0.766150521253197,0.77543890823226,0.802937309949103,0.831097905157373,
0.838009753561634,0.842228568539597,0.84608175125631,0.851031595886933,
0.861874126785413,0.914399762147479,0.942939951596952,0.949203423803074,
0.952041677818635,0.954179832078454,0.956700871283743,0.961219443267498,
0.986776090664185,0.995783710226313,1.02297369908458,1.04190942125654,1.05487675843095,
1.06023618084105,1.06413975890095,1.06823147447015,1.07454732996413,1.09340159334891,
1.13795234375634,1.16608935844108,1.17062746374711,1.17312565637463,1.17528832042572,
1.17812601031381,1.18431452134361,1.21904877008705,1.25299440546504,1.26649418136381,
1.27660561404815,1.28147572109749,1.28530962003881,1.28961705449172,1.29694102868511,
1.32920643338237,1.37072333147956,1.38737691891928),.UNSPECIFIED.);
#1474=B_SPLINE_CURVE_WITH_KNOTS('',3,(#19722,#19723,#19724,#19725),
 .UNSPECIFIED.,.F.,.F.,(4,4),(2.77561970906091,2.77582150461351),
 .UNSPECIFIED.);
#1475=B_SPLINE_CURVE_WITH_KNOTS('',3,(#19726,#19727,#19728,#19729,#19730,
#19731,#19732,#19733,#19734,#19735,#19736,#19737,#19738,#19739,#19740,#19741,
#19742,#19743,#19744,#19745,#19746,#19747,#19748,#19749,#19750,#19751,#19752,
#19753,#19754,#19755,#19756,#19757,#19758,#19759,#19760,#19761,#19762,#19763,
#19764,#19765,#19766,#19767,#19768,#19769,#19770,#19771,#19772,#19773,#19774,
#19775,#19776,#19777,#19778,#19779,#19780,#19781,#19782,#19783,#19784,#19785,
#19786,#19787,#19788,#19789,#19790,#19791,#19792,#19793,#19794,#19795,#19796,
#19797,#19798,#19799,#19800,#19801,#19802,#19803,#19804,#19805,#19806,#19807,
#19808,#19809,#19810,#19811,#19812,#19813,#19814,#19815,#19816,#19817,#19818,
#19819,#19820,#19821,#19822,#19823,#19824,#19825,#19826,#19827,#19828,#19829,
#19830,#19831,#19832,#19833,#19834,#19835,#19836,#19837,#19838,#19839,#19840,
#19841,#19842,#19843,#19844,#19845,#19846,#19847,#19848,#19849,#19850,#19851,
#19852,#19853,#19854,#19855,#19856,#19857,#19858,#19859,#19860,#19861,#19862,
#19863,#19864,#19865,#19866,#19867,#19868,#19869,#19870,#19871,#19872,#19873,
#19874,#19875,#19876,#19877,#19878,#19879,#19880,#19881,#19882,#19883,#19884,
#19885,#19886,#19887,#19888,#19889,#19890,#19891,#19892,#19893,#19894,#19895,
#19896,#19897,#19898,#19899,#19900,#19901,#19902,#19903,#19904,#19905,#19906,
#19907,#19908,#19909,#19910,#19911,#19912,#19913,#19914,#19915,#19916,#19917,
#19918,#19919,#19920,#19921,#19922,#19923,#19924,#19925,#19926,#19927,#19928,
#19929,#19930,#19931),.UNSPECIFIED.,.F.,.F.,(4,2,2,2,2,2,2,2,2,2,2,2,2,
2,2,2,2,2,2,2,2,2,2,2,2,2,2,2,2,2,2,2,2,2,2,2,2,2,2,2,2,2,2,2,2,2,2,2,2,
2,2,2,2,2,2,2,2,2,2,2,2,2,2,2,2,2,2,2,2,2,2,2,2,2,2,2,2,2,2,2,2,2,2,2,2,
2,2,2,2,2,2,2,2,2,2,2,2,2,2,2,2,2,4),(9.71563100416002E-5,0.0442115391377216,
0.0498403619130266,0.052544193992351,0.054467119812325,0.0569573303758112,
0.0614045012205749,0.0850904675135822,0.110413415476681,0.137546768762737,
0.154008548489618,0.159852348687565,0.1638186714502,0.167694952161709,0.173279579473492,
0.186949630735342,0.236491329206391,0.263879455827479,0.270003157766796,
0.272799553069537,0.274914888353178,0.277417100515319,0.281917736768463,
0.307862869991328,0.31706669719401,0.345020856809668,0.372414184984056,
0.379235408779519,0.383407942862652,0.387223860995817,0.39213177292575,
0.400348939950123,0.449683153424383,0.486573954653824,0.491273292128384,
0.493790525812396,0.495924322066288,0.498664899479556,0.504643861572882,
0.545721832064817,0.576672083524734,0.594578097553252,0.600567980979266,
0.604564279601765,0.608418276866243,0.613881145752979,0.626768175537875,
0.676926430237138,0.704718044645319,0.710882786761496,0.713686753829517,
0.715822118362307,0.718327633354895,0.722842634984869,0.749359018366637,
0.757095624674673,0.78356992048174,0.803167726698839,0.816431701565958,
0.821805647930899,0.825682406979315,0.829235449743582,0.834983993314114,
0.849675777432851,0.89805882811185,0.925244918677645,0.931348339078943,
0.934141206365647,0.936275621538627,0.938788905744417,0.943338584868203,
0.971860146414204,1.00005701663801,1.03317765885052,1.0403090465185,1.0445484662088,
1.04834879208563,1.05321242907214,1.06109091535175,1.11413457230855,1.14809163688687,
1.1527061547887,1.15520568838248,1.15734211800294,1.16010830675551,1.16622767810195,
1.20468354465209,1.2373388696191,1.24970912155006,1.25915428411731,1.26386948043372,
1.26762120400276,1.27194228850633,1.27926205245912,1.31936774856166,1.35344834228076,
1.36970336138195,1.37367363508361,1.37603406564585,1.37820866887168,1.3808124063889,
1.38746027865211,1.38751651967754),.UNSPECIFIED.);
#1476=B_SPLINE_CURVE_WITH_KNOTS('',3,(#19933,#19934,#19935,#19936,#19937,
#19938,#19939,#19940,#19941,#19942,#19943,#19944,#19945,#19946,#19947,#19948,
#19949,#19950,#19951,#19952,#19953,#19954,#19955,#19956,#19957,#19958,#19959,
#19960,#19961,#19962,#19963,#19964,#19965,#19966,#19967,#19968,#19969,#19970,
#19971,#19972,#19973,#19974,#19975,#19976,#19977,#19978,#19979,#19980,#19981,
#19982,#19983,#19984,#19985,#19986,#19987,#19988,#19989,#19990,#19991,#19992,
#19993,#19994,#19995,#19996,#19997,#19998,#19999,#20000,#20001,#20002,#20003,
#20004,#20005,#20006,#20007,#20008,#20009,#20010,#20011,#20012,#20013,#20014,
#20015,#20016,#20017,#20018,#20019,#20020,#20021,#20022,#20023,#20024,#20025,
#20026,#20027,#20028,#20029,#20030,#20031,#20032,#20033,#20034,#20035,#20036,
#20037,#20038,#20039,#20040,#20041,#20042,#20043,#20044,#20045,#20046,#20047,
#20048,#20049,#20050,#20051,#20052,#20053,#20054,#20055,#20056,#20057,#20058,
#20059,#20060,#20061,#20062,#20063,#20064,#20065,#20066,#20067,#20068,#20069,
#20070,#20071,#20072,#20073,#20074,#20075,#20076,#20077,#20078,#20079,#20080,
#20081,#20082,#20083,#20084,#20085,#20086,#20087,#20088,#20089,#20090,#20091,
#20092,#20093,#20094,#20095,#20096,#20097,#20098,#20099,#20100,#20101,#20102,
#20103,#20104,#20105,#20106,#20107,#20108,#20109,#20110,#20111,#20112,#20113,
#20114,#20115,#20116,#20117,#20118,#20119,#20120,#20121,#20122,#20123,#20124,
#20125,#20126,#20127,#20128,#20129,#20130,#20131,#20132,#20133,#20134,#20135,
#20136,#20137,#20138),.UNSPECIFIED.,.F.,.F.,(4,2,2,2,2,2,2,2,2,2,2,2,2,
2,2,2,2,2,2,2,2,2,2,2,2,2,2,2,2,2,2,2,2,2,2,2,2,2,2,2,2,2,2,2,2,2,2,2,2,
2,2,2,2,2,2,2,2,2,2,2,2,2,2,2,2,2,2,2,2,2,2,2,2,2,2,2,2,2,2,2,2,2,2,2,2,
2,2,2,2,2,2,2,2,2,2,2,2,2,2,2,2,2,4),(1.38737691891928,1.3874301155379,
1.3914573492088,1.39384492406497,1.39604053387784,1.39915262400335,1.40706582796174,
1.41911011093103,1.46839052997284,1.49253621173924,1.49936766779574,1.50356938820404,
1.50742787565361,1.51249962461698,1.52372725511669,1.55880702423526,1.60221336278169,
1.6097216025008,1.61285967553652,1.6150380628634,1.61740839948999,1.62135732076962,
1.63698676263006,1.67293551647641,1.71178010419775,1.71915389687138,1.72351324060164,
1.72730295139313,1.73207310766056,1.74165901626112,1.75424104973819,1.78780305275641,
1.82471080986153,1.83091250474988,1.83370952547598,1.83586762492197,1.83839232643769,
1.84305578568546,1.87889432823297,1.92949981962921,1.93764213707323,1.94255362866528,
1.94640149050478,1.9506395727265,1.95764169067504,1.98733528312913,2.01356105761642,
2.02023943300273,2.04764620826822,2.05220747199305,2.0547378953764,2.05689495014587,
2.05973076117126,2.06598158750037,2.09439769987869,2.1465210700625,2.15774952630424,
2.16276633134876,2.16662882562305,2.17081518356394,2.17757719804094,2.20350621930206,
2.23278606664219,2.23928866115746,2.26801129224337,2.27258950763136,2.2751236102448,
2.27728000500793,2.280109994405,2.28632924461263,2.31442994759481,2.36558496925798,
2.3774981745826,2.38228337249326,2.38585105711518,2.38978468179788,2.39531611658823,
2.40942752150695,2.43079179498945,2.46969900118903,2.48892417938543,2.49320480741984,
2.49567197196525,2.49784062859814,2.50077990656431,2.50762204299482,2.51749086542158,
2.54926025779796,2.58988411650958,2.59927833908641,2.60407258898838,2.6078985498712,
2.6122524023739,2.61801273761323,2.64168576507317,2.67698879724251,2.70873406769311,
2.71332734559176,2.71586473423071,2.71802059145565,2.72084553106778,2.72703735494925,
2.77453256021917),.UNSPECIFIED.);
#1477=B_SPLINE_CURVE_WITH_KNOTS('',3,(#20139,#20140,#20141,#20142),
 .UNSPECIFIED.,.F.,.F.,(4,4),(0.000109266196132223,0.0003121541379522),
 .UNSPECIFIED.);
#1478=B_SPLINE_CURVE_WITH_KNOTS('',3,(#20147,#20148,#20149,#20150,#20151,
#20152,#20153,#20154,#20155,#20156,#20157,#20158,#20159,#20160,#20161,#20162,
#20163,#20164,#20165,#20166,#20167,#20168,#20169,#20170,#20171,#20172,#20173,
#20174,#20175,#20176,#20177,#20178,#20179,#20180,#20181,#20182,#20183,#20184,
#20185,#20186,#20187,#20188,#20189,#20190,#20191,#20192,#20193,#20194,#20195,
#20196,#20197,#20198,#20199,#20200,#20201,#20202,#20203,#20204,#20205,#20206,
#20207,#20208,#20209,#20210,#20211,#20212,#20213,#20214,#20215,#20216,#20217,
#20218,#20219,#20220,#20221,#20222,#20223,#20224,#20225,#20226,#20227,#20228,
#20229,#20230,#20231,#20232,#20233,#20234,#20235,#20236,#20237,#20238,#20239,
#20240,#20241,#20242,#20243,#20244,#20245,#20246,#20247,#20248,#20249,#20250,
#20251,#20252,#20253,#20254,#20255,#20256,#20257,#20258,#20259,#20260,#20261,
#20262,#20263,#20264,#20265,#20266,#20267,#20268,#20269,#20270,#20271,#20272,
#20273,#20274,#20275,#20276,#20277,#20278,#20279,#20280,#20281,#20282,#20283,
#20284,#20285,#20286,#20287,#20288,#20289,#20290,#20291,#20292,#20293,#20294,
#20295,#20296,#20297,#20298,#20299,#20300,#20301,#20302,#20303,#20304,#20305,
#20306,#20307,#20308,#20309,#20310,#20311,#20312,#20313,#20314,#20315,#20316,
#20317,#20318,#20319,#20320,#20321,#20322,#20323,#20324,#20325,#20326,#20327,
#20328,#20329,#20330,#20331,#20332,#20333,#20334,#20335,#20336,#20337,#20338,
#20339,#20340,#20341,#20342,#20343,#20344,#20345,#20346,#20347,#20348),
 .UNSPECIFIED.,.F.,.F.,(4,2,2,2,2,2,2,2,2,2,2,2,2,2,2,2,2,2,2,2,2,2,2,2,
2,2,2,2,2,2,2,2,2,2,2,2,2,2,2,2,2,2,2,2,2,2,2,2,2,2,2,2,2,2,2,2,2,2,2,2,
2,2,2,2,2,2,2,2,2,2,2,2,2,2,2,2,2,2,2,2,2,2,2,2,2,2,2,2,2,2,2,2,2,2,2,2,
2,2,2,2,4),(1.38831186095198,1.39300679174099,1.39654302199116,1.40043426204388,
1.40589020757036,1.41970332207125,1.4404688199864,1.48145615898468,1.49978162807593,
1.50398918509946,1.50642536965992,1.50857376329047,1.51149230864179,1.51831186933442,
1.5281609251754,1.55992875436192,1.60077237109824,1.61008898947415,1.61484002974374,
1.61862863618847,1.62293605180366,1.63038726635909,1.67615638853852,1.71745784178709,
1.72341109212626,1.72614681219018,1.72828001189852,1.73080036662568,1.73551531377499,
1.77325566367512,1.82162740626428,1.82990849016319,1.83483412721202,1.83865220559887,
1.84281541571348,1.84959467519759,1.87636547945818,1.90494559773848,1.91371259005802,
1.94009986353888,1.94461079538658,1.94711513331963,1.94925020731962,1.95205475132837,
1.9582242477521,1.98606963200391,2.03637985295433,2.04912129632138,2.05456455030475,
2.05841449522715,2.06241497696242,2.06842757892544,2.08653980046283,2.11809508441971,
2.15809186918112,2.16417410500149,2.16693308586477,2.16906823511573,2.17157139552823,
2.17620537796885,2.21228932278736,2.26270968351192,2.2708424605116,2.27572586391455,
2.27953766902553,2.28372089205676,2.29059479451118,2.31884602377331,2.34627971190087,
2.35599762925622,2.38096676790436,2.38544021256849,2.38793599811848,2.39005166421448,
2.39285605519561,2.39902598003031,2.42688019803517,2.47721860213668,2.48992130061587,
2.49535876101637,2.49920726476822,2.50320853121849,2.50922679624455,2.52739391095364,
2.55911443388781,2.59886794325313,2.60494773483509,2.60770603859043,2.60984086209071,
2.6123438830557,2.6169781753519,2.63104405979159,2.66597052296919,2.70614065549259,
2.71350533986767,2.71783525593226,2.72158400700398,2.72628160818939,2.73133113198888,
2.74446638635469,2.77561970906091),.UNSPECIFIED.);
#1479=B_SPLINE_CURVE_WITH_KNOTS('',3,(#20349,#20350,#20351,#20352,#20353,
#20354,#20355,#20356,#20357,#20358,#20359,#20360,#20361,#20362,#20363,#20364,
#20365,#20366,#20367,#20368,#20369,#20370,#20371,#20372,#20373,#20374,#20375,
#20376,#20377,#20378,#20379,#20380,#20381,#20382,#20383,#20384,#20385,#20386,
#20387,#20388,#20389,#20390,#20391,#20392,#20393,#20394,#20395,#20396,#20397,
#20398,#20399,#20400,#20401,#20402,#20403,#20404,#20405,#20406,#20407,#20408,
#20409,#20410,#20411,#20412,#20413,#20414,#20415,#20416,#20417,#20418,#20419,
#20420,#20421,#20422,#20423,#20424,#20425,#20426,#20427,#20428,#20429,#20430,
#20431,#20432,#20433,#20434,#20435,#20436,#20437,#20438,#20439,#20440,#20441,
#20442,#20443,#20444,#20445,#20446,#20447,#20448,#20449,#20450,#20451,#20452,
#20453,#20454,#20455,#20456,#20457,#20458,#20459,#20460,#20461,#20462,#20463,
#20464,#20465,#20466,#20467,#20468,#20469,#20470,#20471,#20472,#20473,#20474,
#20475,#20476,#20477,#20478,#20479,#20480,#20481,#20482,#20483,#20484,#20485,
#20486,#20487,#20488,#20489,#20490,#20491,#20492,#20493,#20494,#20495,#20496,
#20497,#20498,#20499,#20500,#20501,#20502,#20503,#20504,#20505,#20506,#20507,
#20508,#20509,#20510,#20511,#20512,#20513,#20514,#20515,#20516,#20517,#20518,
#20519,#20520,#20521,#20522,#20523,#20524,#20525,#20526,#20527,#20528,#20529,
#20530,#20531,#20532,#20533,#20534,#20535,#20536,#20537,#20538,#20539,#20540,
#20541,#20542,#20543,#20544,#20545,#20546,#20547,#20548,#20549,#20550),
 .UNSPECIFIED.,.F.,.F.,(4,2,2,2,2,2,2,2,2,2,2,2,2,2,2,2,2,2,2,2,2,2,2,2,
2,2,2,2,2,2,2,2,2,2,2,2,2,2,2,2,2,2,2,2,2,2,2,2,2,2,2,2,2,2,2,2,2,2,2,2,
2,2,2,2,2,2,2,2,2,2,2,2,2,2,2,2,2,2,2,2,2,2,2,2,2,2,2,2,2,2,2,2,2,2,2,2,
2,2,2,2,4),(0.0003121541379522,0.0392060648077781,0.0446675046569061,0.0496673000307714,
0.0535160972622554,0.0577520518454449,0.0647432384458444,0.0911778289075277,
0.133032959052139,0.155101639846516,0.159541399983137,0.162018520179388,
0.164185453949274,0.167057699983818,0.173688012089452,0.235750831895649,
0.261197565219785,0.267924910902226,0.272103899441255,0.275968985478701,
0.281002551644563,0.292328410019673,0.344321573823604,0.372693315149619,
0.378939839155464,0.381774885497033,0.383931901223479,0.386462883074088,
0.391026615386072,0.418547368976696,0.425122557310079,0.451354895579256,
0.481068496777416,0.488072081891223,0.492310490273833,0.496158281403396,
0.501069178096886,0.509209322586512,0.559802772661404,0.595619079568649,
0.600281738946522,0.602806255127853,0.604964335404705,0.607761549496186,
0.613964409495356,0.650889101759488,0.684466565962733,0.697052137343631,
0.706639319739503,0.711409643299882,0.71519925888635,0.719558243126607,
0.726930828848786,0.765721436101874,0.79407866111338,0.809278784195776,
0.815623040489877,0.820517129394222,0.823090020178777,0.825242423845138,
0.828019670217397,0.833951279785584,0.875894075120533,0.920832535636686,
0.928423527251669,0.932787580920352,0.936612796362153,0.941393303603974,
0.950719072180697,0.993249719498709,1.02360446460572,1.03323781842868,1.03995921578549,
1.04287803864191,1.04504429410948,1.04752331289461,1.05185555840349,1.07212314259831,
1.11223388723409,1.13219936377714,1.14566068705711,1.15109583943171,1.15501230397639,
1.15908022177954,1.16528432023797,1.18311342917425,1.22854734098628,1.25703573554775,
1.26158218340804,1.26408198040801,1.26624405760627,1.26907845898553,1.27525055637446,
1.30916774530616,1.34370678335913,1.35733268068435,1.36751508693558,1.37239811094477,
1.37623299596259,1.38053196284411,1.38775902368221),.UNSPECIFIED.);
#1480=B_SPLINE_CURVE_WITH_KNOTS('',3,(#20555,#20556,#20557,#20558,#20559,
#20560,#20561,#20562,#20563,#20564,#20565,#20566,#20567,#20568,#20569,#20570,
#20571,#20572,#20573,#20574,#20575,#20576,#20577,#20578,#20579,#20580,#20581,
#20582,#20583,#20584,#20585,#20586,#20587,#20588,#20589,#20590,#20591,#20592,
#20593,#20594,#20595,#20596,#20597,#20598,#20599,#20600,#20601,#20602,#20603,
#20604,#20605,#20606,#20607,#20608,#20609,#20610,#20611,#20612,#20613,#20614,
#20615,#20616,#20617,#20618,#20619,#20620,#20621,#20622,#20623,#20624,#20625,
#20626,#20627,#20628,#20629,#20630,#20631,#20632,#20633,#20634,#20635,#20636,
#20637,#20638,#20639,#20640,#20641,#20642,#20643,#20644,#20645,#20646,#20647,
#20648,#20649,#20650,#20651,#20652,#20653,#20654,#20655,#20656,#20657,#20658,
#20659,#20660,#20661,#20662,#20663,#20664,#20665,#20666,#20667,#20668,#20669,
#20670,#20671,#20672,#20673,#20674,#20675,#20676,#20677,#20678,#20679,#20680,
#20681,#20682,#20683,#20684,#20685,#20686,#20687,#20688,#20689,#20690,#20691,
#20692,#20693,#20694,#20695,#20696,#20697,#20698,#20699,#20700,#20701,#20702,
#20703,#20704,#20705,#20706,#20707,#20708,#20709,#20710,#20711,#20712,#20713,
#20714,#20715,#20716,#20717,#20718,#20719,#20720,#20721,#20722,#20723,#20724,
#20725,#20726,#20727,#20728,#20729,#20730,#20731,#20732,#20733,#20734,#20735,
#20736,#20737,#20738,#20739,#20740,#20741,#20742,#20743,#20744,#20745,#20746,
#20747,#20748,#20749,#20750,#20751,#20752,#20753,#20754,#20755,#20756,#20757,
#20758),.UNSPECIFIED.,.F.,.F.,(4,2,2,2,2,2,2,2,2,2,2,2,2,2,2,2,2,2,2,2,
2,2,2,2,2,2,2,2,2,2,2,2,2,2,2,2,2,2,2,2,2,2,2,2,2,2,2,2,2,2,2,2,2,2,2,2,
2,2,2,2,2,2,2,2,2,2,2,2,2,2,2,2,2,2,2,2,2,2,2,2,2,2,2,2,2,2,2,2,2,2,2,2,
2,2,2,2,2,2,2,2,2,4),(0.000678815151983969,0.0135545168336831,0.0611711635650268,
0.068785317826121,0.0731324065597843,0.0769245232162855,0.0816391428814896,
0.0907550633644243,0.138107932867606,0.164894831513744,0.173869349804587,
0.180121182227087,0.182858732059293,0.182882308764285,0.182906020021552,
0.182929872685781,0.182953873785344,0.185107628733336,0.187548711308559,
0.191771062746313,0.210316627205456,0.249902635531842,0.275918125146367,
0.286838308381199,0.291827560649767,0.295644420915677,0.299820848739743,
0.306655115126896,0.331073289699422,0.372380459411266,0.395378045064019,
0.401024954084468,0.403732281417403,0.405655074684526,0.408140872750035,
0.412572955470426,0.435251989868403,0.474367051463985,0.503042478106631,
0.509939776856481,0.514126327195829,0.517934079849689,0.522802444066866,
0.5308876829993,0.581852597701758,0.616906110202894,0.621887898700021,0.624462163046354,
0.626589763799827,0.629298927888174,0.634955291839129,0.680245073914239,
0.716418150197959,0.72765365234876,0.732697470407692,0.73652112822304,0.740670945791758,
0.747384446099101,0.770356600533664,0.812406110647427,0.836112817095739,
0.841841354491834,0.844564796364056,0.846490187752058,0.848967402473689,
0.853356319456151,0.875118581695272,0.91509631169618,0.943880083691493,
0.950787015088377,0.954977691669364,0.958788172403765,0.963658710019169,
0.971744933331961,1.0226887538672,1.05796650011253,1.06280686867967,1.06535325266426,
1.06748353352322,1.07022964560481,1.07608263647188,1.11922003380121,1.14886726323934,
1.16631302846943,1.17224844112551,1.17623290450731,1.18009378298713,1.18559813203675,
1.19879761270301,1.24865043037431,1.27633816396436,1.28249174220238,1.28529327720863,
1.28740887351293,1.28990710584242,1.2943903513606,1.31968644789017,1.32944596727245,
1.35724538243593,1.3755962880985,1.38825411328145,1.38831186095198),
 .UNSPECIFIED.);
#1481=B_SPLINE_CURVE_WITH_KNOTS('',3,(#20759,#20760,#20761,#20762,#20763,
#20764,#20765,#20766,#20767,#20768,#20769,#20770,#20771,#20772,#20773,#20774,
#20775,#20776,#20777,#20778,#20779,#20780,#20781,#20782,#20783,#20784,#20785,
#20786,#20787,#20788,#20789,#20790,#20791,#20792,#20793,#20794,#20795,#20796,
#20797,#20798,#20799,#20800,#20801,#20802,#20803,#20804,#20805,#20806,#20807,
#20808,#20809,#20810,#20811,#20812,#20813,#20814,#20815,#20816,#20817,#20818,
#20819,#20820,#20821,#20822,#20823,#20824,#20825,#20826,#20827,#20828,#20829,
#20830,#20831,#20832,#20833,#20834,#20835,#20836,#20837,#20838,#20839,#20840,
#20841,#20842,#20843,#20844,#20845,#20846,#20847,#20848,#20849,#20850,#20851,
#20852,#20853,#20854,#20855,#20856,#20857,#20858,#20859,#20860,#20861,#20862,
#20863,#20864,#20865,#20866,#20867,#20868,#20869,#20870,#20871,#20872,#20873,
#20874,#20875,#20876,#20877,#20878,#20879,#20880,#20881,#20882,#20883,#20884,
#20885,#20886,#20887,#20888,#20889,#20890,#20891,#20892,#20893,#20894,#20895,
#20896,#20897,#20898,#20899,#20900,#20901,#20902,#20903,#20904,#20905,#20906,
#20907,#20908,#20909,#20910,#20911,#20912,#20913,#20914,#20915,#20916,#20917,
#20918,#20919,#20920,#20921,#20922,#20923,#20924,#20925,#20926,#20927,#20928,
#20929,#20930,#20931,#20932,#20933,#20934,#20935,#20936,#20937,#20938,#20939,
#20940,#20941,#20942,#20943,#20944,#20945,#20946,#20947,#20948,#20949,#20950,
#20951,#20952,#20953,#20954,#20955,#20956),.UNSPECIFIED.,.F.,.F.,(4,2,2,
2,2,2,2,2,2,2,2,2,2,2,2,2,2,2,2,2,2,2,2,2,2,2,2,2,2,2,2,2,2,2,2,2,2,2,2,
2,2,2,2,2,2,2,2,2,2,2,2,2,2,2,2,2,2,2,2,2,2,2,2,2,2,2,2,2,2,2,2,2,2,2,2,
2,2,2,2,2,2,2,2,2,2,2,2,2,2,2,2,2,2,2,2,2,2,2,4),(1.38775902368221,1.38781776182658,
1.42374712644421,1.44656466883186,1.47725592566392,1.48184182100099,1.48437775373741,
1.48653408692494,1.48936189250973,1.4955684715692,1.52354014058484,1.5743016397036,
1.58655876987782,1.59141817215752,1.59500391331784,1.59892126356546,1.60436186837484,
1.6178600672121,1.63790158758803,1.67939432613439,1.69823860898585,1.70249993736081,
1.70496283476324,1.70713275010269,1.71008047812879,1.71697163238382,1.72693585378422,
1.7592944092514,1.79921455801226,1.80858355382043,1.81337288105224,1.81719873071807,
1.82155657174777,1.82911871885237,1.87480171672228,1.91592657861927,1.92191200258405,
1.92469921463186,1.92685229858058,1.92941758616548,1.93427494944176,1.97198056740512,
2.02004914483874,2.02837280105711,2.03333556913017,2.03719035569486,2.04140239587713,
2.04828353353468,2.07596800873124,2.10365331108819,2.11318871315535,2.13859625795144,
2.14310994963642,2.14562968799694,2.14776750608049,2.15060643345803,2.15687600065352,
2.18548625751486,2.23821952923997,2.24875309821462,2.25371951467301,2.25757419174051,
2.26178313377423,2.26865234096921,2.29616551954454,2.3239479129378,2.33320957629621,
2.35896443119481,2.36348692724304,2.36600838321833,2.36814574978579,2.37098143808224,
2.37723304271062,2.40566134282915,2.45782418080421,2.46901476055243,2.47402475321731,
2.47788594508415,2.4820748041927,2.48884966745186,2.51496670806313,2.54395636565273,
2.57667707315928,2.58285036238085,2.58568481360637,2.5878469686997,2.59018570910623,
2.59419563317155,2.59933803021425,2.61043454439731,2.64995370249589,2.68430283169248,
2.69168464554774,2.69600421555137,2.69945254035975,2.70411374928957,2.713144566244,
2.74595194315684,2.77514791930297),.UNSPECIFIED.);
#1482=B_SPLINE_CURVE_WITH_KNOTS('',3,(#20962,#20963,#20964,#20965,#20966,
#20967,#20968,#20969,#20970,#20971,#20972,#20973,#20974,#20975,#20976,#20977,
#20978,#20979,#20980,#20981,#20982,#20983,#20984,#20985,#20986,#20987,#20988,
#20989,#20990,#20991,#20992,#20993,#20994,#20995,#20996,#20997,#20998,#20999,
#21000,#21001,#21002,#21003,#21004,#21005,#21006,#21007,#21008,#21009,#21010,
#21011,#21012,#21013,#21014,#21015,#21016,#21017,#21018,#21019,#21020,#21021,
#21022,#21023,#21024,#21025,#21026,#21027,#21028,#21029,#21030,#21031,#21032,
#21033,#21034,#21035,#21036,#21037,#21038,#21039,#21040,#21041,#21042,#21043,
#21044,#21045,#21046,#21047,#21048,#21049,#21050,#21051,#21052,#21053,#21054,
#21055,#21056,#21057,#21058,#21059,#21060,#21061,#21062,#21063,#21064,#21065,
#21066,#21067,#21068,#21069,#21070,#21071,#21072,#21073,#21074,#21075,#21076,
#21077,#21078,#21079,#21080,#21081,#21082,#21083,#21084,#21085,#21086,#21087,
#21088,#21089,#21090,#21091,#21092,#21093,#21094,#21095,#21096,#21097,#21098,
#21099,#21100,#21101,#21102,#21103,#21104,#21105,#21106,#21107,#21108,#21109,
#21110,#21111),.UNSPECIFIED.,.F.,.F.,(4,2,2,2,2,2,2,2,2,2,2,2,2,2,2,2,2,
2,2,2,2,2,2,2,2,2,2,2,2,2,2,2,2,2,2,2,2,2,2,2,2,2,2,2,2,2,2,2,2,2,2,2,2,
2,2,2,2,2,2,2,2,2,2,2,2,2,2,2,2,2,2,2,2,2,4),(-0.875860537968119,-0.875799606618078,
-0.873773553177765,-0.87149818754001,-0.867965548349446,-0.856448447729897,
-0.833732991281093,-0.799161880436857,-0.7917731182112,-0.787046992948174,
-0.783221389412492,-0.778784941286976,-0.770787706902226,-0.743813012619747,
-0.714534998448861,-0.702085142336867,-0.698351752718789,-0.696031594790346,
-0.69375930589405,-0.690263543538742,-0.679161910350972,-0.657871591932514,
-0.621533610623069,-0.614210117781182,-0.609499808353657,-0.605670060507595,
-0.601209419402849,-0.593111931121542,-0.565409806606647,-0.534782653391671,
-0.524105848956321,-0.520558385012711,-0.518505374981075,-0.51627358885697,
-0.512907823993746,-0.502797067005756,-0.48459875051324,-0.442538530977189,
-0.434986466049484,-0.430616436242226,-0.426812791679861,-0.422068984773143,
-0.412400073099503,-0.387174926820729,-0.356300434820293,-0.3459572784027,
-0.342459350338071,-0.340421463188156,-0.338162941301972,-0.334728984138968,
-0.324197280876602,-0.304782797605587,-0.265008585893149,-0.257163635100863,
-0.2526991700981,-0.248854362295849,-0.244110087804886,-0.234613342481773,
-0.20863912342285,-0.176848272932624,-0.167766002900717,-0.164404377275654,
-0.162165968466191,-0.159749783833764,-0.155725018712719,-0.138391996764361,
-0.116508694397701,-0.0871482397750525,-0.0803511701143885,-0.076130777917414,
-0.0722018029327749,-0.066922343944156,-0.0544148358211864,-0.0357514952089097,
-8.33018978494207E-5),.UNSPECIFIED.);
#1483=B_SPLINE_CURVE_WITH_KNOTS('',3,(#21114,#21115,#21116,#21117,#21118,
#21119,#21120,#21121,#21122,#21123,#21124,#21125,#21126,#21127,#21128,#21129,
#21130,#21131,#21132,#21133,#21134,#21135,#21136,#21137,#21138,#21139,#21140,
#21141,#21142,#21143,#21144,#21145,#21146,#21147,#21148,#21149,#21150,#21151,
#21152,#21153,#21154,#21155,#21156,#21157,#21158,#21159,#21160,#21161,#21162,
#21163,#21164,#21165,#21166,#21167,#21168,#21169,#21170,#21171,#21172,#21173,
#21174,#21175,#21176,#21177,#21178,#21179,#21180,#21181,#21182,#21183,#21184,
#21185,#21186,#21187,#21188,#21189,#21190,#21191,#21192,#21193,#21194,#21195,
#21196,#21197,#21198,#21199,#21200,#21201,#21202,#21203,#21204,#21205,#21206,
#21207,#21208,#21209,#21210,#21211,#21212,#21213,#21214,#21215,#21216,#21217,
#21218,#21219,#21220,#21221,#21222,#21223,#21224,#21225,#21226,#21227,#21228,
#21229,#21230,#21231,#21232,#21233,#21234,#21235,#21236,#21237,#21238,#21239,
#21240,#21241,#21242,#21243,#21244,#21245,#21246,#21247,#21248,#21249,#21250,
#21251,#21252,#21253,#21254,#21255),.UNSPECIFIED.,.F.,.F.,(4,3,3,3,3,3,
3,3,3,3,3,3,3,3,3,3,3,3,3,3,3,3,3,3,3,3,3,3,3,3,3,3,3,3,3,3,3,3,3,3,3,3,
3,3,3,3,3,4),(16.7019922841306,16.8021818348996,16.8124544772726,16.9234210411684,
17.033796869599,17.1441744311209,17.2545854631975,17.3659858445079,17.4766375907132,
17.5884122895762,17.6885982648488,17.7001869884391,17.7002311104944,17.7964751471802,
17.8072802155964,17.9128977895231,17.9186679002403,18.0254288144202,18.1321132984658,
18.2387615669814,18.3454137772225,18.4521802784855,18.5590147146697,18.6591545584869,
18.6660336585631,18.6983816927476,18.6984356183394,18.7948863424963,18.8065090728564,
18.9177674883813,19.025595407644,19.1333563054358,19.2410888397907,19.3488316227747,
19.4566913005886,19.5646218816293,19.6655852004633,19.6727314597256,19.6965763970561,
19.6966231841011,19.7936651766023,19.8047706499335,19.912813978709,20.0207451306855,
20.1286177204737,20.2364557658273,20.3443346961532,20.3930532338378),
 .UNSPECIFIED.);
#1484=B_SPLINE_CURVE_WITH_KNOTS('',3,(#21260,#21261,#21262,#21263,#21264,
#21265,#21266,#21267,#21268,#21269,#21270,#21271,#21272,#21273,#21274,#21275,
#21276,#21277,#21278,#21279,#21280,#21281,#21282,#21283,#21284,#21285,#21286,
#21287,#21288,#21289,#21290,#21291,#21292,#21293,#21294,#21295,#21296,#21297,
#21298,#21299,#21300,#21301,#21302,#21303,#21304,#21305,#21306,#21307,#21308,
#21309,#21310,#21311,#21312,#21313,#21314,#21315,#21316,#21317,#21318,#21319,
#21320,#21321,#21322,#21323,#21324,#21325,#21326,#21327,#21328,#21329,#21330,
#21331,#21332,#21333,#21334,#21335,#21336,#21337,#21338,#21339,#21340,#21341,
#21342,#21343,#21344,#21345,#21346,#21347,#21348,#21349,#21350,#21351,#21352,
#21353,#21354,#21355,#21356,#21357,#21358,#21359,#21360,#21361,#21362,#21363,
#21364,#21365,#21366,#21367,#21368,#21369,#21370,#21371,#21372,#21373,#21374,
#21375,#21376,#21377,#21378,#21379,#21380,#21381,#21382,#21383,#21384,#21385,
#21386,#21387,#21388,#21389,#21390,#21391,#21392,#21393,#21394,#21395,#21396,
#21397,#21398,#21399,#21400,#21401,#21402,#21403,#21404,#21405,#21406,#21407,
#21408,#21409,#21410,#21411,#21412,#21413,#21414,#21415,#21416,#21417,#21418,
#21419,#21420,#21421,#21422,#21423,#21424,#21425,#21426,#21427,#21428,#21429,
#21430,#21431,#21432,#21433,#21434,#21435,#21436,#21437,#21438,#21439,#21440,
#21441,#21442,#21443),.UNSPECIFIED.,.F.,.F.,(4,2,2,2,2,2,2,2,2,2,2,2,2,
2,2,2,2,2,2,2,2,2,2,2,2,2,2,2,2,2,2,2,2,2,2,2,2,2,2,2,2,2,2,2,2,2,2,2,2,
2,2,2,2,2,2,2,2,2,2,2,2,2,2,2,2,2,2,2,2,2,2,2,2,2,2,2,2,2,2,2,2,2,2,2,2,
2,2,2,2,2,2,4),(-1.99499716658925,-1.96752270825511,-1.94735063860436,-1.9432359106537,
-1.94083476043791,-1.93864780433138,-1.93596208580319,-1.92934417914976,
-1.8905985110623,-1.8722417129216,-1.85992088737411,-1.85471003307461,-1.8508313424147,
-1.84666657370522,-1.83997068590978,-1.81348594212233,-1.78232516918049,
-1.77318699572475,-1.76683405113085,-1.76399298440067,-1.76183078296909,
-1.75923191431716,-1.75432223774033,-1.71877759529623,-1.68657481614049,
-1.67927563000575,-1.67498453647151,-1.67114167156058,-1.66619958340817,
-1.65552021073062,-1.61175799810463,-1.59818907533202,-1.58980992138503,
-1.58665154432093,-1.58444856108206,-1.58202640779601,-1.57781376053967,
-1.55697423009811,-1.50949969125568,-1.50186736047801,-1.49746427033655,
-1.49363844392233,-1.48887447161339,-1.47918665538803,-1.4540281706685,
-1.42324846697106,-1.41279424097747,-1.40927380511322,-1.40722622457644,
-1.40497445531411,-1.40155505405732,-1.39109638873522,-1.37187045168249,
-1.33199521259349,-1.32420786483485,-1.31977091427651,-1.31594741940937,
-1.31122721591586,-1.30177611565075,-1.27091861601456,-1.2380028042242,
-1.23287399570558,-1.23022887746032,-1.2282859390128,-1.22561845713784,
-1.22021226502215,-1.19806621687394,-1.15657997283186,-1.14740409230815,
-1.14267694825044,-1.13885217487448,-1.13441853589904,-1.12643178956738,
-1.09953739031325,-1.07044095700247,-1.05772019663939,-1.05396507648837,
-1.05164182429368,-1.04938381387754,-1.04592827264721,-1.03512785458699,
-1.01482501961887,-0.976708412160299,-0.969463684150646,-0.964782683476268,
-0.960964021124115,-0.956502357916562,-0.948363876558926,-0.92025785255302,
-0.888782192695983,-0.879208177009835,-0.875860537968119),.UNSPECIFIED.);
#1485=B_SPLINE_CURVE_WITH_KNOTS('',3,(#21444,#21445,#21446,#21447,#21448,
#21449,#21450,#21451,#21452,#21453,#21454,#21455,#21456,#21457,#21458,#21459,
#21460,#21461,#21462,#21463,#21464,#21465,#21466,#21467,#21468,#21469,#21470,
#21471,#21472,#21473,#21474,#21475,#21476,#21477,#21478,#21479,#21480,#21481,
#21482,#21483,#21484,#21485,#21486,#21487,#21488,#21489,#21490,#21491,#21492,
#21493,#21494,#21495,#21496,#21497,#21498,#21499,#21500,#21501,#21502,#21503,
#21504,#21505,#21506,#21507,#21508,#21509,#21510,#21511,#21512,#21513,#21514,
#21515,#21516,#21517,#21518,#21519,#21520,#21521,#21522,#21523,#21524,#21525,
#21526,#21527,#21528,#21529,#21530,#21531,#21532,#21533,#21534,#21535,#21536,
#21537,#21538,#21539,#21540,#21541,#21542,#21543,#21544,#21545,#21546,#21547,
#21548,#21549,#21550,#21551,#21552,#21553,#21554,#21555,#21556,#21557,#21558,
#21559,#21560,#21561,#21562,#21563,#21564,#21565,#21566,#21567,#21568,#21569,
#21570,#21571,#21572,#21573,#21574,#21575,#21576,#21577,#21578,#21579,#21580,
#21581,#21582,#21583,#21584,#21585,#21586,#21587,#21588,#21589,#21590,#21591,
#21592,#21593,#21594,#21595,#21596,#21597,#21598,#21599,#21600,#21601,#21602,
#21603,#21604,#21605,#21606,#21607,#21608,#21609,#21610,#21611,#21612,#21613,
#21614,#21615,#21616,#21617,#21618,#21619,#21620,#21621,#21622,#21623,#21624,
#21625,#21626,#21627,#21628,#21629,#21630,#21631),.UNSPECIFIED.,.F.,.F.,
(4,2,2,2,2,2,2,2,2,2,2,2,2,2,2,2,2,2,2,2,2,2,2,2,2,2,2,2,2,2,2,2,2,2,2,
2,2,2,2,2,2,2,2,2,2,2,2,2,2,2,2,2,2,2,2,2,2,2,2,2,2,2,2,2,2,2,2,2,2,2,2,
2,2,2,2,2,2,2,2,2,2,2,2,2,2,2,2,2,2,2,2,2,2,4),(-5.59315610037617,-5.55336009091651,
-5.54468070666692,-5.54149575826921,-5.53930355215932,-5.53694214376124,
-5.53290593997252,-5.51564082705649,-5.48516821989026,-5.46958897838822,
-5.46199122264363,-5.45571624027886,-5.45183829629559,-5.44804344453449,
-5.44313686827759,-5.43206746069107,-5.39235075299744,-5.37067543905196,
-5.36535666667643,-5.36273451778536,-5.3608201428546,-5.35821291898656,
-5.35302769445264,-5.32043304297661,-5.28490221519477,-5.27799207685714,
-5.27380635635698,-5.26998139760904,-5.26503810849382,-5.25388108299712,
-5.21458055505209,-5.19314176132561,-5.18783107528596,-5.18519453495156,
-5.18326905299212,-5.18064249491269,-5.17536672417524,-5.13521978947001,
-5.10917482210811,-5.10133472572026,-5.09695938027789,-5.09317362824814,
-5.08848166764673,-5.08111969262822,-5.04668957869126,-5.02380202938147,
-5.01598141826372,-5.01032649433526,-5.00762902801662,-5.00549607300724,
-5.00283538453111,-4.99736863056442,-4.9711948142544,-4.94608375823654,
-4.92778764252021,-4.92186448637815,-4.91789012705217,-4.91401980341187,
-4.90931936558815,-4.8976438120184,-4.85898282298198,-4.83771786023274,
-4.83243255025401,-4.82980711646114,-4.82788687276963,-4.82526442917046,
-4.82000164325571,-4.77977013837314,-4.75374368839018,-4.74590586747846,
-4.74153148252857,-4.73774643581759,-4.73305518618399,-4.72569380318942,
-4.69152347916303,-4.66849914427294,-4.66065422490463,-4.65498618095219,
-4.65228564625593,-4.65015133546778,-4.64748991070208,-4.64202587343494,
-4.61469886284387,-4.57810890277073,-4.56907203287847,-4.56446021409638,
-4.56104690657797,-4.55674919128219,-4.5494722161337,-4.50572686508456,
-4.48854084273066,-4.47879510090985,-4.47547992283627,-4.4747574653027),
 .UNSPECIFIED.);
#1486=B_SPLINE_CURVE_WITH_KNOTS('',3,(#21637,#21638,#21639,#21640),
 .UNSPECIFIED.,.F.,.F.,(4,4),(-8.84127953393321E-6,-1.00000008615431E-6),
 .UNSPECIFIED.);
#1487=B_SPLINE_CURVE_WITH_KNOTS('',3,(#21641,#21642,#21643,#21644,#21645,
#21646,#21647,#21648,#21649,#21650,#21651,#21652,#21653,#21654,#21655,#21656,
#21657,#21658,#21659,#21660,#21661,#21662,#21663,#21664,#21665,#21666,#21667,
#21668,#21669,#21670,#21671,#21672,#21673,#21674,#21675,#21676,#21677,#21678,
#21679,#21680,#21681,#21682,#21683,#21684,#21685,#21686,#21687,#21688,#21689,
#21690,#21691,#21692,#21693,#21694,#21695,#21696,#21697,#21698,#21699,#21700,
#21701,#21702,#21703,#21704,#21705,#21706,#21707,#21708,#21709,#21710,#21711,
#21712,#21713,#21714,#21715,#21716,#21717,#21718,#21719,#21720,#21721,#21722,
#21723,#21724,#21725,#21726,#21727,#21728,#21729,#21730,#21731,#21732,#21733,
#21734,#21735,#21736,#21737,#21738,#21739,#21740,#21741,#21742,#21743,#21744,
#21745,#21746,#21747,#21748,#21749,#21750,#21751,#21752,#21753,#21754,#21755,
#21756,#21757,#21758,#21759,#21760,#21761,#21762,#21763,#21764,#21765,#21766,
#21767,#21768,#21769,#21770,#21771,#21772,#21773,#21774,#21775,#21776,#21777,
#21778,#21779,#21780,#21781,#21782,#21783,#21784,#21785,#21786,#21787,#21788,
#21789,#21790,#21791,#21792,#21793,#21794,#21795,#21796,#21797,#21798,#21799,
#21800,#21801,#21802,#21803,#21804,#21805,#21806,#21807,#21808,#21809,#21810,
#21811,#21812,#21813,#21814,#21815,#21816,#21817,#21818,#21819,#21820,#21821,
#21822,#21823,#21824,#21825,#21826,#21827,#21828,#21829,#21830,#21831,#21832,
#21833,#21834,#21835,#21836,#21837,#21838,#21839,#21840),.UNSPECIFIED.,
 .F.,.F.,(4,2,2,2,2,2,2,2,2,2,2,2,2,2,2,2,2,2,2,2,2,2,2,2,2,2,2,2,2,2,2,
2,2,2,2,2,2,2,2,2,2,2,2,2,2,2,2,2,2,2,2,2,2,2,2,2,2,2,2,2,2,2,2,2,2,2,2,
2,2,2,2,2,2,2,2,2,2,2,2,2,2,2,2,2,2,2,2,2,2,2,2,2,2,2,2,2,2,2,2,4),(-3.1139997766405,
-3.10786717358469,-3.10313095141403,-3.09929576443767,-3.09566140548508,
-3.09159150592066,-3.08535274331309,-3.06560943062476,-3.04529385652988,
-3.02394341873807,-3.01282322641162,-3.00933168828933,-3.00706504947068,
-3.00503078088594,-3.00158186315971,-2.99170530925925,-2.96049510615426,
-2.93252725611136,-2.92440373088149,-2.91994304339184,-2.91612119592423,
-2.91143107643737,-2.90416139239354,-2.86639798284569,-2.84586666879241,
-2.83499470172268,-2.83152959464521,-2.82926842461164,-2.82722936680897,
-2.82375482122616,-2.81367552186303,-2.78262519304721,-2.75473697020179,
-2.74662346945896,-2.742164791089,-2.73834279398468,-2.73365012307323,-2.7263717616517,
-2.68875306615179,-2.66812854152223,-2.65722786518841,-2.65375964940731,
-2.65149782745637,-2.64917701533559,-2.64543292634974,-2.63283416350648,
-2.60367433854199,-2.57675289645067,-2.56876351241746,-2.56433002413462,
-2.56050627987812,-2.55578162480459,-2.54839345627139,-2.51393502074948,
-2.4911397523198,-2.47960166400224,-2.47606703124804,-2.47379131745189,
-2.471764323461,-2.46835507398318,-2.4587849946654,-2.4273297117135,-2.39923979742529,
-2.39110080403027,-2.38663692546834,-2.38281517452671,-2.37812874833993,
-2.37087190275465,-2.33290063946706,-2.31250068666943,-2.30166922582491,
-2.29820844583645,-2.29594813130233,-2.29362531824098,-2.28987216823794,
-2.27717131240512,-2.27320829484086,-2.22345287285724,-2.21407461879421,
-2.20936838870713,-2.20554594345223,-2.20109867669856,-2.19326244784376,
-2.15385099969815,-2.13433545748308,-2.12378359464746,-2.12035372517665,
-2.11809986380834,-2.11605428501288,-2.11254461890502,-2.10217914219586,
-2.07135506493894,-2.06673609042256,-2.04283669872105,-2.03516634509768,
-2.03079850454282,-2.0269685232856,-2.02215328350044,-2.01218671374677,
-1.99499716658925),.UNSPECIFIED.);
#1488=B_SPLINE_CURVE_WITH_KNOTS('',3,(#21841,#21842,#21843,#21844,#21845,
#21846,#21847,#21848,#21849,#21850,#21851,#21852,#21853,#21854,#21855,#21856,
#21857,#21858,#21859,#21860,#21861,#21862,#21863,#21864,#21865,#21866,#21867,
#21868,#21869,#21870,#21871,#21872,#21873,#21874,#21875,#21876,#21877,#21878,
#21879,#21880,#21881,#21882,#21883,#21884,#21885,#21886,#21887,#21888,#21889,
#21890,#21891,#21892,#21893,#21894,#21895,#21896,#21897,#21898,#21899,#21900,
#21901,#21902,#21903,#21904,#21905,#21906,#21907,#21908,#21909,#21910,#21911,
#21912,#21913,#21914,#21915,#21916,#21917,#21918,#21919,#21920,#21921,#21922,
#21923,#21924,#21925,#21926,#21927,#21928,#21929,#21930,#21931,#21932,#21933,
#21934,#21935,#21936,#21937,#21938,#21939,#21940,#21941,#21942,#21943,#21944,
#21945,#21946,#21947,#21948,#21949,#21950,#21951,#21952,#21953,#21954,#21955,
#21956,#21957,#21958,#21959,#21960,#21961,#21962,#21963,#21964,#21965,#21966,
#21967,#21968,#21969,#21970,#21971,#21972,#21973,#21974,#21975,#21976,#21977,
#21978,#21979,#21980,#21981,#21982,#21983,#21984,#21985,#21986,#21987,#21988,
#21989,#21990,#21991,#21992,#21993,#21994,#21995,#21996,#21997,#21998,#21999,
#22000,#22001,#22002,#22003,#22004,#22005,#22006,#22007,#22008,#22009,#22010,
#22011,#22012,#22013,#22014,#22015,#22016,#22017,#22018,#22019,#22020,#22021,
#22022,#22023,#22024,#22025,#22026,#22027,#22028,#22029,#22030,#22031,#22032),
 .UNSPECIFIED.,.F.,.F.,(4,2,2,2,2,2,2,2,2,2,2,2,2,2,2,2,2,2,2,2,2,2,2,2,
2,2,2,2,2,2,2,2,2,2,2,2,2,2,2,2,2,2,2,2,2,2,2,2,2,2,2,2,2,2,2,2,2,2,2,2,
2,2,2,2,2,2,2,2,2,2,2,2,2,2,2,2,2,2,2,2,2,2,2,2,2,2,2,2,2,2,2,2,2,2,2,4),
(-4.4747574653027,-4.47326539155446,-4.47122679992775,-4.46767864801904,
-4.45680377328828,-4.41412104218659,-4.39490205505733,-4.38888742570857,
-4.38489290809498,-4.3810332425115,-4.37638271074941,-4.36492125697367,
-4.32601974773498,-4.30467944294444,-4.29938452696129,-4.2967560851514,
-4.2948350970118,-4.29221360519118,-4.28695518095048,-4.24670484063484,
-4.22069337965014,-4.21285851551769,-4.20848541952633,-4.20470132826991,
-4.20001110713729,-4.19265121097419,-4.15835777417686,-4.13540421342134,
-4.1275724521397,-4.12191176580497,-4.11921322559772,-4.1170795142747,-4.11441772629565,
-4.10895077624916,-4.08385939488568,-4.05503519514153,-4.04412763514328,
-4.03565801431279,-4.03115696044226,-4.02775233398908,-4.02336644618819,
-4.01568406543595,-3.97510161814073,-3.95622494312453,-3.94590171752278,
-3.94251912163939,-3.94029108632671,-3.93798411401097,-3.93423136146072,
-3.92126178096673,-3.89236486843817,-3.86555605105747,-3.85761566658606,
-3.85322103576581,-3.84943864518334,-3.84477658997144,-3.83751353172781,
-3.8001699924732,-3.77932563528012,-3.7683795602408,-3.76492862796063,-3.76268651608166,
-3.76039736082186,-3.7567269193915,-3.74468139024641,-3.71511917927646,
-3.68796447362976,-3.67997903474244,-3.67557515280169,-3.67179326185878,
-3.66714258339532,-3.65819841061653,-3.61641981939016,-3.59414338260762,
-3.58874711982154,-3.5860987480815,-3.58417668339503,-3.58157344791445,
-3.57640847159548,-3.54345083467954,-3.51260411806326,-3.50319337517041,
-3.49851044195156,-3.49472661487203,-3.49034758989789,-3.48269789941469,
-3.44182256874747,-3.42310799143732,-3.41283808599623,-3.40946136119019,
-3.40723438459369,-3.40492550709695,-3.40116458074908,-3.38810295257325,
-3.35926906550475,-3.35634983843352),.UNSPECIFIED.);
#1489=B_SPLINE_CURVE_WITH_KNOTS('',3,(#22037,#22038,#22039,#22040,#22041,
#22042,#22043,#22044,#22045,#22046,#22047,#22048,#22049,#22050,#22051,#22052,
#22053,#22054,#22055,#22056,#22057,#22058,#22059,#22060,#22061,#22062,#22063,
#22064,#22065,#22066,#22067,#22068,#22069,#22070,#22071,#22072,#22073,#22074,
#22075,#22076,#22077,#22078,#22079,#22080,#22081,#22082,#22083,#22084,#22085,
#22086,#22087,#22088,#22089,#22090,#22091,#22092,#22093,#22094,#22095,#22096,
#22097,#22098,#22099,#22100,#22101,#22102,#22103,#22104,#22105,#22106,#22107,
#22108,#22109,#22110,#22111,#22112,#22113,#22114,#22115,#22116,#22117,#22118,
#22119,#22120,#22121,#22122,#22123,#22124,#22125,#22126,#22127,#22128,#22129,
#22130,#22131,#22132,#22133,#22134,#22135,#22136,#22137,#22138,#22139,#22140,
#22141,#22142,#22143,#22144,#22145,#22146,#22147,#22148,#22149,#22150,#22151,
#22152,#22153,#22154,#22155,#22156,#22157,#22158,#22159,#22160,#22161,#22162,
#22163,#22164,#22165,#22166,#22167,#22168,#22169,#22170,#22171,#22172,#22173,
#22174,#22175,#22176,#22177,#22178,#22179,#22180,#22181,#22182,#22183,#22184,
#22185,#22186,#22187,#22188,#22189,#22190,#22191,#22192,#22193,#22194,#22195,
#22196,#22197,#22198,#22199,#22200,#22201,#22202,#22203,#22204,#22205,#22206,
#22207,#22208,#22209,#22210,#22211,#22212,#22213,#22214,#22215,#22216,#22217,
#22218,#22219,#22220,#22221,#22222),.UNSPECIFIED.,.F.,.F.,(4,2,2,2,2,2,
2,2,2,2,2,2,2,2,2,2,2,2,2,2,2,2,2,2,2,2,2,2,2,2,2,2,2,2,2,2,2,2,2,2,2,2,
2,2,2,2,2,2,2,2,2,2,2,2,2,2,2,2,2,2,2,2,2,2,2,2,2,2,2,2,2,2,2,2,2,2,2,2,
2,2,2,2,2,2,2,2,2,2,2,2,2,2,4),(-1.11918234038498,-1.1062908624538,-1.06420020199838,
-1.05627401622338,-1.05139521280838,-1.04755932581885,-1.04323193802121,
-1.03575732258743,-1.00271471962037,-0.968524114009293,-0.963473507625799,
-0.960844958582337,-0.958901819449467,-0.956218385220644,-0.950725822975816,
-0.927750625134705,-0.883950830818214,-0.87657163698206,-0.87226411565372,
-0.868424820339599,-0.86351270814788,-0.853003765437371,-0.803674626480437,
-0.788656202161589,-0.784710120192069,-0.782345369193335,-0.780113669352325,
-0.776797017681588,-0.767212956474858,-0.750534316864445,-0.708116258644078,
-0.700428817531146,-0.695617705790056,-0.691787629430989,-0.687416035342625,
-0.679729294925883,-0.670155629469278,-0.647579385029872,-0.612791185148299,
-0.607796077431028,-0.605179093552806,-0.603039120201972,-0.600233812846179,
-0.594083704099069,-0.585344457961139,-0.557023668584067,-0.527243108045143,
-0.520442165931277,-0.51625523206506,-0.512384276309439,-0.507226873978072,
-0.495249455226615,-0.477644726311858,-0.443805892544685,-0.432447097693965,
-0.428822092930933,-0.426754044593035,-0.424520151581741,-0.421192464504828,
-0.411519187864713,-0.39459337576055,-0.350426382462267,-0.343098662258047,
-0.338801493034557,-0.334959624219661,-0.330027807099145,-0.31940840349828,
-0.304598944901089,-0.282825937345396,-0.25790938238555,-0.252417953672966,
-0.249734617132589,-0.247577320518606,-0.244837547162199,-0.239047116623659,
-0.230994916129851,-0.206918960243676,-0.174327126996468,-0.166872391128234,
-0.162128208701056,-0.158302974491009,-0.153883642006941,-0.145964835264397,
-0.136010036494511,-0.11182885421081,-0.0797644168535668,-0.0745062912994022,
-0.0718682101913314,-0.0699253668840754,-0.0672516767516004,-0.0618106216543333,
-0.039332013226959,-8.84127953393321E-6),.UNSPECIFIED.);
#1490=B_SPLINE_CURVE_WITH_KNOTS('',3,(#22223,#22224,#22225,#22226,#22227,
#22228,#22229,#22230,#22231,#22232,#22233,#22234,#22235,#22236,#22237,#22238,
#22239,#22240,#22241,#22242,#22243,#22244,#22245,#22246,#22247,#22248,#22249,
#22250,#22251,#22252,#22253,#22254,#22255,#22256,#22257,#22258,#22259,#22260,
#22261,#22262,#22263,#22264,#22265,#22266,#22267,#22268,#22269,#22270,#22271,
#22272,#22273,#22274,#22275,#22276,#22277,#22278,#22279,#22280,#22281,#22282,
#22283,#22284,#22285,#22286,#22287,#22288,#22289,#22290,#22291,#22292,#22293,
#22294,#22295,#22296,#22297,#22298,#22299,#22300,#22301,#22302,#22303,#22304,
#22305,#22306,#22307,#22308,#22309,#22310,#22311,#22312,#22313,#22314,#22315,
#22316,#22317,#22318,#22319,#22320,#22321,#22322,#22323,#22324,#22325,#22326,
#22327,#22328,#22329,#22330,#22331,#22332,#22333,#22334,#22335,#22336,#22337,
#22338,#22339,#22340,#22341,#22342,#22343,#22344,#22345,#22346,#22347,#22348,
#22349,#22350,#22351,#22352,#22353,#22354,#22355,#22356,#22357,#22358,#22359,
#22360,#22361,#22362,#22363,#22364,#22365,#22366,#22367,#22368,#22369,#22370,
#22371,#22372,#22373,#22374,#22375,#22376,#22377,#22378,#22379,#22380,#22381,
#22382,#22383,#22384,#22385,#22386,#22387,#22388,#22389,#22390,#22391,#22392,
#22393,#22394,#22395,#22396,#22397,#22398,#22399,#22400,#22401,#22402,#22403,
#22404,#22405,#22406,#22407,#22408,#22409,#22410,#22411,#22412,#22413,#22414),
 .UNSPECIFIED.,.F.,.F.,(4,2,2,2,2,2,2,2,2,2,2,2,2,2,2,2,2,2,2,2,2,2,2,2,
2,2,2,2,2,2,2,2,2,2,2,2,2,2,2,2,2,2,2,2,2,2,2,2,2,2,2,2,2,2,2,2,2,2,2,2,
2,2,2,2,2,2,2,2,2,2,2,2,2,2,2,2,2,2,2,2,2,2,2,2,2,2,2,2,2,2,2,2,2,2,2,4),
(-3.35634983843352,-3.33249191080876,-3.32455529168109,-3.32016118668897,
-3.31637840165538,-3.31171477689914,-3.30444709018579,-3.2671791475581,
-3.24628183255185,-3.2353193185757,-3.23186644442745,-3.22962379602355,
-3.22733487510822,-3.2236660359991,-3.21163975151283,-3.18206062530389,
-3.15489621736199,-3.14690919416847,-3.14250478707676,-3.13872263380292,
-3.13407187330001,-3.12512831994961,-3.08334466617103,-3.0610658601259,
-3.05566912152535,-3.05302054362203,-3.05109833720453,-3.04849492273822,
-3.04332965330926,-3.00258951258646,-2.9768437089507,-2.96904407031554,
-2.96467787150807,-2.96089270125881,-2.95619201711199,-2.94879706414001,
-2.91718389978793,-2.89224067494513,-2.88405638900473,-2.87820788855236,
-2.8754743670322,-2.87333958130688,-2.87070933097621,-2.86540692544813,
-2.83384428254287,-2.8224081209352,-2.79672242669935,-2.79023351091857,
-2.78614060281697,-2.7822914187972,-2.77706359857726,-2.76442006374167,
-2.74528137378472,-2.70564058946459,-2.70026041146983,-2.69761497718234,
-2.69548054824832,-2.69276357168621,-2.68700532126765,-2.67899245898068,
-2.65503443361358,-2.62214256050429,-2.61475891585796,-2.61006131419861,
-2.60627610830684,-2.60190708367343,-2.59409467479844,-2.56825612461192,
-2.52763087623772,-2.52243623028852,-2.5198268483335,-2.51790470266971,
-2.51526191133981,-2.50989606232597,-2.4879102617746,-2.447037421138,-2.43720688756629,
-2.43244579988985,-2.42865572756464,-2.4243312998688,-2.41673605326765,
-2.3836629341208,-2.34976520886268,-2.34471029969662,-2.34209653468647,
-2.3401745632025,-2.33753633207052,-2.33219414470639,-2.31042880111988,
-2.27023699617197,-2.25978802510393,-2.25491632441335,-2.25111555742662,
-2.24685972821094,-2.23959477212428,-2.23775823947936),.UNSPECIFIED.);
#1491=B_SPLINE_CURVE_WITH_KNOTS('',3,(#22419,#22420,#22421,#22422,#22423,
#22424,#22425,#22426,#22427,#22428,#22429,#22430,#22431,#22432,#22433,#22434,
#22435,#22436,#22437,#22438,#22439,#22440,#22441,#22442,#22443,#22444,#22445,
#22446,#22447,#22448,#22449,#22450,#22451,#22452,#22453,#22454,#22455,#22456,
#22457,#22458,#22459,#22460,#22461,#22462,#22463,#22464,#22465,#22466,#22467,
#22468,#22469,#22470,#22471,#22472,#22473,#22474,#22475,#22476,#22477,#22478,
#22479,#22480,#22481,#22482,#22483,#22484,#22485,#22486,#22487,#22488,#22489,
#22490,#22491,#22492,#22493,#22494,#22495,#22496,#22497,#22498,#22499,#22500,
#22501,#22502,#22503,#22504,#22505,#22506,#22507,#22508,#22509,#22510,#22511,
#22512,#22513,#22514,#22515,#22516,#22517,#22518,#22519,#22520,#22521,#22522,
#22523,#22524,#22525,#22526,#22527,#22528,#22529,#22530,#22531,#22532,#22533,
#22534,#22535,#22536,#22537,#22538,#22539,#22540,#22541,#22542,#22543,#22544,
#22545,#22546,#22547,#22548,#22549,#22550,#22551,#22552,#22553,#22554,#22555,
#22556,#22557,#22558,#22559,#22560,#22561,#22562,#22563,#22564,#22565,#22566,
#22567,#22568,#22569,#22570,#22571,#22572,#22573,#22574,#22575,#22576,#22577,
#22578,#22579,#22580,#22581,#22582,#22583,#22584,#22585,#22586,#22587,#22588,
#22589,#22590,#22591,#22592,#22593,#22594,#22595,#22596,#22597,#22598,#22599,
#22600,#22601,#22602,#22603,#22604,#22605,#22606,#22607,#22608,#22609,#22610),
 .UNSPECIFIED.,.F.,.F.,(4,2,2,2,2,2,2,2,2,2,2,2,2,2,2,2,2,2,2,2,2,2,2,2,
2,2,2,2,2,2,2,2,2,2,2,2,2,2,2,2,2,2,2,2,2,2,2,2,2,2,2,2,2,2,2,2,2,2,2,2,
2,2,2,2,2,2,2,2,2,2,2,2,2,2,2,2,2,2,2,2,2,2,2,2,2,2,2,2,2,2,2,2,2,2,2,4),
(-2.23814687865753,-2.2135431078615,-2.20804974798867,-2.20536657571047,
-2.20321000138374,-2.20047189255,-2.19468748382366,-2.1866456685039,-2.16262154776817,
-2.12990913544601,-2.12249567916594,-2.11776430486937,-2.11394103106288,
-2.10951466569314,-2.10155691898455,-2.07486862763743,-2.04616187342406,
-2.03291166967119,-2.02911129195532,-2.0267786393877,-2.02452685343346,
-2.0211059684685,-2.01063017848018,-1.99134830012102,-1.95159310831359,
-1.94379698917397,-1.93935884234044,-1.93553647479024,-1.93082042781496,
-1.92138755723278,-1.89177308604314,-1.85744923063672,-1.85241202228884,
-1.84978662012121,-1.84784373937883,-1.84515802270196,-1.83965176070333,
-1.81653727947187,-1.77297414864555,-1.76556388724565,-1.76125047510115,
-1.75741319039678,-1.75251366649491,-1.74207275704226,-1.69288029668137,
-1.67766390183171,-1.67370623712585,-1.67133929058727,-1.669109649141,-1.66580200733089,
-1.65628719905207,-1.63979698948903,-1.59813526220858,-1.58909658117665,
-1.58439817327087,-1.5805763911687,-1.57612348144307,-1.56803660795203,
-1.54035334711031,-1.50971775893567,-1.4990832645134,-1.49554139263011,
-1.49348975882711,-1.49124221506284,-1.48784319704305,-1.47756225508325,
-1.45887454988745,-1.41806791807798,-1.41038578606383,-1.40597196746985,
-1.40214721171164,-1.39739805934924,-1.38778977758836,-1.33790151248559,
-1.32215719264125,-1.31816544950352,-1.31579094371483,-1.31356521581295,
-1.3102792001932,-1.30093901363295,-1.28492342671935,-1.2451205505612,-1.23536506023486,
-1.23052833364272,-1.22695015784882,-1.22301506120958,-1.21746655173353,
-1.20277306521964,-1.17853868090279,-1.14658116786608,-1.14131027314233,
-1.13866985603365,-1.13672734415375,-1.13405671890653,-1.12863065038081,
-1.11918234038498),.UNSPECIFIED.);
#1492=B_SPLINE_CURVE_WITH_KNOTS('',3,(#22611,#22612,#22613,#22614,#22615,
#22616,#22617,#22618,#22619,#22620,#22621,#22622,#22623,#22624,#22625,#22626,
#22627,#22628,#22629,#22630,#22631,#22632,#22633,#22634,#22635,#22636,#22637,
#22638,#22639,#22640,#22641,#22642,#22643,#22644,#22645,#22646,#22647,#22648,
#22649,#22650,#22651,#22652,#22653,#22654,#22655,#22656,#22657,#22658,#22659,
#22660,#22661,#22662,#22663,#22664,#22665,#22666,#22667,#22668,#22669,#22670,
#22671,#22672,#22673,#22674,#22675,#22676,#22677,#22678,#22679,#22680,#22681,
#22682,#22683,#22684,#22685,#22686,#22687,#22688,#22689,#22690,#22691,#22692,
#22693,#22694,#22695,#22696,#22697,#22698,#22699,#22700,#22701,#22702,#22703,
#22704,#22705,#22706,#22707,#22708,#22709,#22710,#22711,#22712,#22713,#22714,
#22715,#22716,#22717,#22718,#22719,#22720,#22721,#22722,#22723,#22724,#22725,
#22726,#22727,#22728,#22729,#22730,#22731,#22732,#22733,#22734,#22735,#22736,
#22737,#22738,#22739,#22740,#22741,#22742,#22743,#22744,#22745,#22746,#22747,
#22748,#22749,#22750,#22751,#22752,#22753,#22754,#22755,#22756,#22757,#22758,
#22759,#22760,#22761,#22762,#22763,#22764,#22765,#22766,#22767,#22768,#22769,
#22770,#22771,#22772,#22773,#22774,#22775,#22776,#22777,#22778,#22779,#22780,
#22781,#22782,#22783,#22784,#22785,#22786,#22787,#22788,#22789,#22790,#22791,
#22792,#22793,#22794,#22795,#22796,#22797,#22798,#22799,#22800),
 .UNSPECIFIED.,.F.,.F.,(4,2,2,2,2,2,2,2,2,2,2,2,2,2,2,2,2,2,2,2,2,2,2,2,
2,2,2,2,2,2,2,2,2,2,2,2,2,2,2,2,2,2,2,2,2,2,2,2,2,2,2,2,2,2,2,2,2,2,2,2,
2,2,2,2,2,2,2,2,2,2,2,2,2,2,2,2,2,2,2,2,2,2,2,2,2,2,2,2,2,2,2,2,2,2,4),
(-2.23775823947936,-2.2306787948275,-2.2105876527433,-2.18011911248231,
-2.16924918976833,-2.16570076042661,-2.16366166535568,-2.16144630879085,
-2.15812929492565,-2.14837256766464,-2.13115878676025,-2.08749980007724,
-2.08021312644081,-2.07591269632872,-2.07249887310717,-2.06788847036118,
-2.0588624911135,-2.04698567050094,-2.01247995750546,-1.9926756173253,-1.98852576555277,
-1.98613240962921,-1.98395183348138,-1.98082381188729,-1.97252310223593,
-1.95910552436682,-1.9165349388954,-1.90514840551939,-1.90049182036467,
-1.89662966389264,-1.89263516732375,-1.88662572169422,-1.86748055483274,
-1.82533821083558,-1.81390114510191,-1.81028946515461,-1.80801262562257,
-1.80575850450113,-1.80225267106759,-1.7907813747335,-1.76814683167503,
-1.73342280059525,-1.72607107304305,-1.72138244339194,-1.71759742518013,
-1.71322080996329,-1.70537284397219,-1.6792730193121,-1.63910470544662,
-1.63382059367302,-1.63119350726861,-1.62905801915656,-1.62631944488431,
-1.62044562902757,-1.61221500631695,-1.58699756023594,-1.55576771034777,
-1.54837114322118,-1.54366931039112,-1.53988316331238,-1.53551577810844,
-1.5277139365101,-1.50195977508585,-1.46116523836969,-1.45600131709839,
-1.45339769021933,-1.45147485976189,-1.44882485331593,-1.44342322560829,
-1.4211066069806,-1.37919425383731,-1.37113871850652,-1.36624892683847,
-1.36244561540714,-1.35819883426958,-1.35097941392647,-1.34213654353765,
-1.32231980853656,-1.29254539552005,-1.28073916766702,-1.27709020096959,
-1.27480512246437,-1.27255785141656,-1.26908529886751,-1.25794164288413,
-1.23644403402488,-1.20008984650402,-1.19278206877593,-1.18810591875068,
-1.18432126212414,-1.17993424150091,-1.17203691232783,-1.14556943797177,
-1.12769927842475,-1.11895968873475),.UNSPECIFIED.);
#1493=B_SPLINE_CURVE_WITH_KNOTS('',3,(#22805,#22806,#22807,#22808,#22809,
#22810,#22811,#22812,#22813,#22814,#22815,#22816,#22817,#22818,#22819,#22820,
#22821,#22822,#22823,#22824,#22825,#22826,#22827,#22828,#22829,#22830,#22831,
#22832,#22833,#22834,#22835,#22836,#22837,#22838,#22839,#22840,#22841,#22842,
#22843,#22844,#22845,#22846,#22847,#22848,#22849,#22850,#22851,#22852,#22853,
#22854,#22855,#22856,#22857,#22858,#22859,#22860,#22861,#22862,#22863,#22864,
#22865,#22866,#22867,#22868,#22869,#22870,#22871,#22872,#22873,#22874,#22875,
#22876,#22877,#22878,#22879,#22880,#22881,#22882,#22883,#22884,#22885,#22886,
#22887,#22888,#22889,#22890,#22891,#22892,#22893,#22894,#22895,#22896,#22897,
#22898,#22899,#22900,#22901,#22902,#22903,#22904,#22905,#22906,#22907,#22908,
#22909,#22910,#22911,#22912,#22913,#22914,#22915,#22916,#22917,#22918,#22919,
#22920,#22921,#22922,#22923,#22924,#22925,#22926,#22927,#22928,#22929,#22930,
#22931,#22932,#22933,#22934,#22935,#22936,#22937,#22938,#22939,#22940,#22941,
#22942,#22943,#22944,#22945,#22946,#22947,#22948,#22949,#22950,#22951,#22952,
#22953,#22954,#22955,#22956,#22957,#22958,#22959,#22960,#22961,#22962,#22963,
#22964,#22965,#22966,#22967,#22968,#22969,#22970,#22971,#22972,#22973,#22974,
#22975,#22976,#22977,#22978,#22979,#22980,#22981,#22982,#22983,#22984,#22985,
#22986,#22987,#22988,#22989,#22990,#22991,#22992,#22993,#22994),
 .UNSPECIFIED.,.F.,.F.,(4,2,2,2,2,2,2,2,2,2,2,2,2,2,2,2,2,2,2,2,2,2,2,2,
2,2,2,2,2,2,2,2,2,2,2,2,2,2,2,2,2,2,2,2,2,2,2,2,2,2,2,2,2,2,2,2,2,2,2,2,
2,2,2,2,2,2,2,2,2,2,2,2,2,2,2,2,2,2,2,2,2,2,2,2,2,2,2,2,2,2,2,2,2,2,4),
(-3.35683790262814,-3.35357765786577,-3.34585385121407,-3.30540077861235,
-3.28649997223239,-3.27614956588511,-3.27274304308916,-3.27049436269867,
-3.26815809506247,-3.26434029196816,-3.25091460056561,-3.22236500958243,
-3.19576253352604,-3.18781654161179,-3.18339289860963,-3.17956985962477,
-3.17483605044204,-3.16741316655585,-3.13591493929963,-3.1109545636412,
-3.10275006563831,-3.09688004221786,-3.09412626871319,-3.09196954141775,
-3.08930129384187,-3.08388457979645,-3.05546727072702,-3.01756402987333,
-3.00989126300549,-3.00552378902994,-3.00169511871894,-2.99688284316519,
-2.98692744605904,-2.94617547786139,-2.92425662202074,-2.9188764450497,
-2.91621523552983,-2.91427372240898,-2.91162602237495,-2.90631523604085,
-2.87469984863652,-2.85032156290244,-2.83557786716483,-2.83002403064476,
-2.82608886051902,-2.82203695599074,-2.81588172154763,-2.79710827897907,
-2.7558213741243,-2.74361411904854,-2.73990586470275,-2.73759322536519,
-2.73532576603829,-2.7318285505923,-2.72064779064818,-2.69908882023927,
-2.66293184755867,-2.6555916381664,-2.65088158260726,-2.64705959878097,
-2.6426168781004,-2.63457859630774,-2.60727072001866,-2.57736886295229,
-2.56577349884824,-2.56212375171917,-2.55982375040387,-2.55754508321889,
-2.55399474610088,-2.54229238651305,-2.51889807746939,-2.48532678589276,
-2.47792585839745,-2.47319812513326,-2.46937508068943,-2.4649459590731,
-2.45697466345485,-2.43018299542566,-2.40127561086429,-2.38830531401297,
-2.38452922840036,-2.38220185035745,-2.37994612356052,-2.37650585629217,
-2.36585589829144,-2.34603131104018,-2.30719074307194,-2.29930748410362,
-2.29485059465778,-2.29102945865006,-2.28633699380245,-2.27702906079664,
-2.26467859484985,-2.2396455148825,-2.23814687865753),.UNSPECIFIED.);
#1494=B_SPLINE_CURVE_WITH_KNOTS('',3,(#22995,#22996,#22997,#22998,#22999,
#23000,#23001,#23002,#23003,#23004,#23005,#23006,#23007,#23008,#23009,#23010,
#23011,#23012,#23013,#23014,#23015,#23016,#23017,#23018,#23019,#23020,#23021,
#23022,#23023,#23024,#23025,#23026,#23027,#23028,#23029,#23030,#23031,#23032,
#23033,#23034,#23035,#23036,#23037,#23038,#23039,#23040,#23041,#23042,#23043,
#23044,#23045,#23046,#23047,#23048,#23049,#23050,#23051,#23052,#23053,#23054,
#23055,#23056,#23057,#23058,#23059,#23060,#23061,#23062,#23063,#23064,#23065,
#23066,#23067,#23068,#23069,#23070,#23071,#23072,#23073,#23074,#23075,#23076,
#23077,#23078,#23079,#23080,#23081,#23082,#23083,#23084,#23085,#23086,#23087,
#23088,#23089,#23090,#23091,#23092,#23093,#23094,#23095,#23096,#23097,#23098,
#23099,#23100,#23101,#23102,#23103,#23104,#23105,#23106,#23107,#23108,#23109,
#23110,#23111,#23112,#23113,#23114,#23115,#23116,#23117,#23118,#23119,#23120,
#23121,#23122,#23123,#23124,#23125,#23126,#23127,#23128,#23129,#23130,#23131,
#23132,#23133,#23134,#23135,#23136,#23137,#23138,#23139,#23140,#23141,#23142,
#23143,#23144,#23145,#23146,#23147,#23148,#23149,#23150,#23151,#23152,#23153,
#23154,#23155,#23156,#23157,#23158,#23159,#23160,#23161,#23162,#23163,#23164,
#23165,#23166,#23167,#23168,#23169,#23170,#23171,#23172,#23173,#23174,#23175,
#23176,#23177,#23178,#23179,#23180,#23181,#23182,#23183,#23184,#23185,#23186,
#23187,#23188,#23189,#23190,#23191,#23192),.UNSPECIFIED.,.F.,.F.,(4,2,2,
2,2,2,2,2,2,2,2,2,2,2,2,2,2,2,2,2,2,2,2,2,2,2,2,2,2,2,2,2,2,2,2,2,2,2,2,
2,2,2,2,2,2,2,2,2,2,2,2,2,2,2,2,2,2,2,2,2,2,2,2,2,2,2,2,2,2,2,2,2,2,2,2,
2,2,2,2,2,2,2,2,2,2,2,2,2,2,2,2,2,2,2,2,2,2,2,4),(-1.11895968873475,-1.10411380111841,
-1.09987897483287,-1.09746713616499,-1.09529327166464,-1.09220743431856,
-1.08420511429452,-1.0714953711734,-1.04717908954595,-1.01976971294961,
-1.01309028604818,-1.00895664090545,-1.00512207966775,-0.999995394948391,
-0.9880161445331,-0.970362031004053,-0.936280333397552,-0.92513958812141,
-0.921560035703689,-0.919514596591889,-0.917303792701365,-0.914011914746847,
-0.904466028681687,-0.887843517248697,-0.845775033507896,-0.837836200575998,
-0.832979129487298,-0.82917924137921,-0.824913466164491,-0.817603579294294,
-0.808616297437559,-0.788259925821318,-0.757115212264873,-0.747107063254117,
-0.743661421783218,-0.741641684244542,-0.7394064691808,-0.735992283748977,
-0.725394661679828,-0.705677430006427,-0.666548097173002,-0.658715262066274,
-0.654295701276274,-0.650513021992327,-0.645877390033169,-0.63672301006463,
-0.598906937911911,-0.572919279484284,-0.567445527887247,-0.564781622198941,
-0.562646897977396,-0.559947963286475,-0.554289180390262,-0.546463185408821,
-0.523546856591881,-0.489203837333374,-0.481842564093089,-0.477150685114914,
-0.473364807398216,-0.468989154277872,-0.461148427261187,-0.435108798969085,
-0.394817519824743,-0.389554406945539,-0.386931120857671,-0.385008961842906,
-0.382379103688018,-0.377082322774433,-0.355741782665113,-0.316839225126266,
-0.305377376396611,-0.300724980334268,-0.2968630274758,-0.292865396152958,
-0.286844604131098,-0.267591960181098,-0.224762765940421,-0.213969068077737,
-0.210428582884749,-0.208390538184037,-0.206172796356866,-0.202846521691293,
-0.193018887126509,-0.175607474683788,-0.132306006357323,-0.124964642422751,
-0.120651266930897,-0.117237626708801,-0.112641038413573,-0.103692208073208,
-0.0822647593686294,-0.0506571534242049,-0.0367799085092122,-0.032937057104142,
-0.0306096245284612,-0.0283934190696086,-0.0261254434108124,-0.0228906791297862,
-9.99999999695689E-7),.UNSPECIFIED.);
#1495=B_SPLINE_CURVE_WITH_KNOTS('',3,(#23197,#23198,#23199,#23200,#23201,
#23202,#23203,#23204,#23205,#23206,#23207,#23208,#23209,#23210,#23211,#23212,
#23213,#23214,#23215,#23216,#23217,#23218,#23219,#23220,#23221,#23222,#23223,
#23224,#23225,#23226,#23227,#23228,#23229,#23230,#23231,#23232,#23233,#23234,
#23235,#23236,#23237,#23238,#23239,#23240,#23241,#23242,#23243,#23244,#23245,
#23246,#23247,#23248,#23249,#23250,#23251,#23252,#23253,#23254,#23255,#23256,
#23257,#23258,#23259,#23260,#23261,#23262,#23263,#23264,#23265,#23266,#23267,
#23268,#23269,#23270,#23271,#23272,#23273,#23274,#23275,#23276,#23277,#23278,
#23279,#23280,#23281,#23282,#23283,#23284,#23285,#23286,#23287,#23288,#23289,
#23290,#23291,#23292,#23293,#23294,#23295,#23296,#23297,#23298,#23299,#23300,
#23301,#23302,#23303,#23304,#23305,#23306,#23307,#23308,#23309,#23310,#23311,
#23312,#23313,#23314,#23315,#23316,#23317,#23318,#23319,#23320,#23321,#23322,
#23323,#23324,#23325,#23326,#23327,#23328,#23329,#23330,#23331,#23332,#23333,
#23334,#23335,#23336,#23337,#23338,#23339,#23340,#23341,#23342,#23343,#23344,
#23345,#23346,#23347,#23348,#23349,#23350,#23351,#23352,#23353,#23354,#23355,
#23356,#23357,#23358,#23359,#23360,#23361,#23362,#23363,#23364,#23365,#23366,
#23367,#23368,#23369,#23370,#23371,#23372,#23373,#23374,#23375,#23376,#23377,
#23378,#23379,#23380,#23381,#23382,#23383,#23384,#23385,#23386,#23387,#23388,
#23389,#23390,#23391,#23392),.UNSPECIFIED.,.F.,.F.,(4,2,2,2,2,2,2,2,2,2,
2,2,2,2,2,2,2,2,2,2,2,2,2,2,2,2,2,2,2,2,2,2,2,2,2,2,2,2,2,2,2,2,2,2,2,2,
2,2,2,2,2,2,2,2,2,2,2,2,2,2,2,2,2,2,2,2,2,2,2,2,2,2,2,2,2,2,2,2,2,2,2,2,
2,2,2,2,2,2,2,2,2,2,2,2,2,2,2,4),(-4.47528237196998,-4.47047723035589,-4.43862345421251,
-4.4312285888014,-4.42691966002181,-4.42308370713672,-4.41818221954144,
-4.41016934329169,-4.36820404056406,-4.34590397795295,-4.34048409174089,
-4.3378157277645,-4.33587452597949,-4.3332353725376,-4.32812921860268,-4.29484950989231,
-4.28497268168759,-4.26785736398973,-4.25610986305653,-4.25099165077918,
-4.24712864214056,-4.24292962605829,-4.23606122298278,-4.20572274378787,
-4.18298967547927,-4.16578720960486,-4.16181891012491,-4.15945043105863,
-4.15724954140713,-4.15397333850673,-4.14538372350735,-4.11315834756111,
-4.09242577625489,-4.08332116277573,-4.07592473331271,-4.07161520210312,
-4.06777889623146,-4.06287721053346,-4.05241771468118,-4.01223373781848,
-3.99050106477531,-3.98514170141821,-3.98248491664646,-3.98054400310775,
-3.97789324705692,-3.97256485030836,-3.94187253896268,-3.92933592293723,
-3.90919293646593,-3.89969165200108,-3.89496369824028,-3.89114171457042,
-3.886715201937,-3.87896920685487,-3.83202710892516,-3.81076579878064,-3.8066108135089,
-3.80420169204174,-3.80201968343461,-3.79885226936393,-3.79278801431145,
-3.75398211121775,-3.73562319673773,-3.72716513418025,-3.72017563747995,
-3.7159506928184,-3.71209442869865,-3.7071159046257,-3.69589560817632,-3.65651494500333,
-3.64060826556114,-3.63425811958733,-3.62941417039701,-3.62685997629127,
-3.62469330883092,-3.62184137798591,-3.61524293862453,-3.58112647403818,
-3.55421202871605,-3.5444187757795,-3.53963622105286,-3.5358449858793,-3.53147003892715,
-3.5239638531155,-3.48172499313599,-3.46380297773179,-3.45378220980638,
-3.45041386536529,-3.44817282362102,-3.4461153458794,-3.44254138099382,
-3.43162595691448,-3.39740648965698,-3.37609716138104,-3.36655839977513,
-3.36182292304886,-3.35799986058677,-3.35683790262814),.UNSPECIFIED.);
#1496=B_SPLINE_CURVE_WITH_KNOTS('',3,(#23393,#23394,#23395,#23396,#23397,
#23398,#23399,#23400,#23401,#23402,#23403,#23404,#23405,#23406,#23407,#23408,
#23409,#23410,#23411,#23412,#23413,#23414,#23415,#23416,#23417,#23418,#23419,
#23420,#23421,#23422,#23423,#23424,#23425,#23426,#23427,#23428,#23429,#23430,
#23431,#23432,#23433,#23434,#23435,#23436,#23437,#23438,#23439,#23440,#23441,
#23442,#23443,#23444,#23445,#23446,#23447,#23448,#23449,#23450,#23451,#23452,
#23453,#23454,#23455,#23456,#23457,#23458,#23459,#23460,#23461,#23462,#23463,
#23464,#23465,#23466,#23467,#23468,#23469,#23470,#23471,#23472,#23473,#23474,
#23475,#23476,#23477,#23478,#23479,#23480,#23481,#23482,#23483,#23484,#23485,
#23486,#23487,#23488,#23489,#23490,#23491,#23492,#23493,#23494,#23495,#23496,
#23497,#23498,#23499,#23500,#23501,#23502,#23503,#23504,#23505,#23506,#23507,
#23508,#23509,#23510,#23511,#23512,#23513,#23514,#23515,#23516,#23517,#23518,
#23519,#23520,#23521,#23522,#23523,#23524,#23525,#23526,#23527,#23528,#23529,
#23530,#23531,#23532,#23533,#23534,#23535,#23536,#23537,#23538,#23539,#23540,
#23541,#23542,#23543,#23544,#23545,#23546,#23547,#23548,#23549,#23550,#23551,
#23552,#23553,#23554,#23555,#23556,#23557,#23558,#23559,#23560,#23561,#23562,
#23563,#23564,#23565,#23566,#23567,#23568,#23569,#23570,#23571,#23572,#23573,
#23574),.UNSPECIFIED.,.F.,.F.,(4,2,2,2,2,2,2,2,2,2,2,2,2,2,2,2,2,2,2,2,
2,2,2,2,2,2,2,2,2,2,2,2,2,2,2,2,2,2,2,2,2,2,2,2,2,2,2,2,2,2,2,2,2,2,2,2,
2,2,2,2,2,2,2,2,2,2,2,2,2,2,2,2,2,2,2,2,2,2,2,2,2,2,2,2,2,2,2,2,2,2,4),
(-5.87804291519136,-5.83428954882498,-5.82829041028316,-5.82294371139109,
-5.81907490801547,-5.81550538548975,-5.80963855698751,-5.79334671522187,
-5.75865981592281,-5.74436672223993,-5.73578386261734,-5.73280426955157,
-5.73057178090971,-5.72827007924657,-5.72454245732517,-5.71186594800043,
-5.68276522388351,-5.65583554927645,-5.64787886969071,-5.64348057715903,
-5.6396979335013,-5.63503926031245,-5.62605695335963,-5.58431836518343,
-5.5620534799279,-5.55665815010132,-5.55400980969516,-5.55208757616313,
-5.54948383284988,-5.5443170746154,-5.50358300320923,-5.47783277690756,
-5.47003244416382,-5.46566604134631,-5.46188079631145,-5.45718015171272,
-5.4476761320721,-5.40641244311933,-5.38429743054231,-5.37891796515281,
-5.37627265464834,-5.37435053032704,-5.3717438696003,-5.36656247948738,
-5.32590154556352,-5.30010996779205,-5.29230396448624,-5.28793634411328,
-5.28415112530444,-5.27945191620595,-5.27206242725214,-5.23952580457398,
-5.21527610276786,-5.20721117918484,-5.20142578494464,-5.19870381434753,
-5.19656930218491,-5.19392852014822,-5.1885722263864,-5.15862408070966,
-5.12462702874218,-5.11549139675546,-5.11086024345266,-5.10707884573524,
-5.10265808316319,-5.09481585154511,-5.05578815584266,-5.0359972321654,
-5.0253775937572,-5.0219615698462,-5.01972644842878,-5.01742789985704,-5.01371512856654,
-5.00120823539113,-4.97197344022922,-4.94498753853897,-4.93702333926827,
-4.93262338654208,-4.92884066508907,-4.92418361562163,-4.91520998264583,
-4.87345860958561,-4.85118928593465,-4.84579334459361,-4.84314481144704,
-4.84122248507763,-4.83861868496744,-4.83345201237418,-4.79271438968909,
-4.76696387829719,-4.7594056615118),.UNSPECIFIED.);
#1497=B_SPLINE_CURVE_WITH_KNOTS('',3,(#23579,#23580,#23581,#23582,#23583,
#23584,#23585,#23586,#23587,#23588,#23589,#23590,#23591,#23592,#23593,#23594,
#23595,#23596,#23597,#23598,#23599,#23600,#23601,#23602,#23603,#23604,#23605,
#23606,#23607,#23608,#23609,#23610,#23611,#23612,#23613,#23614,#23615,#23616,
#23617,#23618,#23619,#23620,#23621,#23622,#23623,#23624,#23625,#23626,#23627,
#23628,#23629,#23630,#23631,#23632,#23633,#23634,#23635,#23636,#23637,#23638,
#23639,#23640,#23641,#23642,#23643,#23644,#23645,#23646,#23647,#23648,#23649,
#23650,#23651,#23652,#23653,#23654,#23655,#23656,#23657,#23658,#23659,#23660,
#23661,#23662,#23663,#23664,#23665,#23666,#23667,#23668,#23669,#23670,#23671,
#23672,#23673,#23674,#23675,#23676,#23677,#23678,#23679,#23680,#23681,#23682,
#23683,#23684,#23685,#23686,#23687,#23688,#23689,#23690,#23691,#23692,#23693,
#23694,#23695,#23696,#23697,#23698,#23699,#23700,#23701,#23702,#23703,#23704,
#23705,#23706,#23707,#23708,#23709,#23710,#23711,#23712,#23713,#23714,#23715,
#23716,#23717,#23718,#23719,#23720,#23721,#23722,#23723,#23724,#23725,#23726,
#23727,#23728,#23729,#23730,#23731,#23732,#23733,#23734,#23735,#23736,#23737,
#23738,#23739,#23740,#23741,#23742,#23743,#23744,#23745,#23746,#23747,#23748,
#23749,#23750,#23751,#23752,#23753,#23754,#23755,#23756,#23757,#23758,#23759,
#23760,#23761,#23762,#23763,#23764,#23765,#23766,#23767,#23768,#23769,#23770,
#23771,#23772),.UNSPECIFIED.,.F.,.F.,(4,2,2,2,2,2,2,2,2,2,2,2,2,2,2,2,2,
2,2,2,2,2,2,2,2,2,2,2,2,2,2,2,2,2,2,2,2,2,2,2,2,2,2,2,2,2,2,2,2,2,2,2,2,
2,2,2,2,2,2,2,2,2,2,2,2,2,2,2,2,2,2,2,2,2,2,2,2,2,2,2,2,2,2,2,2,2,2,2,2,
2,2,2,2,2,2,2,4),(-5.59347479354677,-5.58807672447325,-5.58435005752554,
-5.58212670041714,-5.58008295740095,-5.57771331531301,-5.57373863595134,
-5.55820622565288,-5.53272755108873,-5.50561552972491,-5.49760493978463,
-5.49316936137948,-5.48934906854456,-5.48463540563768,-5.4772780294438,
-5.44177303429365,-5.41975774612149,-5.40844599917441,-5.40493631486158,
-5.40266706912718,-5.40035913339524,-5.39666901672206,-5.38464048325009,
-5.35509884269625,-5.32798821861477,-5.31997777097135,-5.31554219737878,
-5.31172186855447,-5.30700810989418,-5.29965048052116,-5.26415229808797,
-5.24213182981134,-5.23081854038086,-5.22730867691153,-5.22503938040182,
-5.22301030220606,-5.21958369115782,-5.20986766975057,-5.17855977522271,
-5.1505528619324,-5.14242792885165,-5.13796910805751,-5.13415027008705,
-5.12946562572585,-5.12220797647264,-5.08436854797338,-5.06391983137564,
-5.05307682654478,-5.04961659819174,-5.04735761613324,-5.04503721383123,
-5.04128965961214,-5.02862871070675,-4.99954302071318,-4.97538888975385,
-4.96575233058842,-4.96099979415817,-4.95717698050517,-4.95277054711678,
-4.9451147238471,-4.90171911749374,-4.87898361711773,-4.87351808336627,
-4.87084099033883,-4.86889946118434,-4.86626868776896,-4.86120223923617,
-4.82730798027529,-4.79342366251387,-4.78631404860024,-4.78206472161939,
-4.77821628183218,-4.77328954451502,-4.76237520202226,-4.7226860216023,
-4.70111672781088,-4.69577545993641,-4.69312237978978,-4.69096580656558,
-4.68819678079606,-4.6822404680028,-4.64253983138402,-4.62406030050576,
-4.61168744557028,-4.60647096795489,-4.60259365871226,-4.59843558921065,
-4.59176214847682,-4.56585748649067,-4.53423326734789,-4.52503823731938,
-4.51865789027738,-4.51581332248875,-4.51365233107255,-4.51105966357998,
-4.5061733925627,-4.47528237196998),.UNSPECIFIED.);
#1498=B_SPLINE_CURVE_WITH_KNOTS('',3,(#23773,#23774,#23775,#23776,#23777,
#23778,#23779,#23780,#23781,#23782,#23783,#23784,#23785,#23786,#23787,#23788,
#23789,#23790,#23791,#23792,#23793,#23794,#23795,#23796,#23797,#23798,#23799,
#23800,#23801,#23802,#23803,#23804,#23805,#23806,#23807,#23808,#23809,#23810,
#23811,#23812,#23813,#23814,#23815,#23816,#23817,#23818,#23819,#23820,#23821,
#23822,#23823,#23824,#23825,#23826,#23827,#23828,#23829,#23830,#23831,#23832,
#23833,#23834,#23835,#23836,#23837,#23838,#23839,#23840,#23841,#23842,#23843,
#23844,#23845,#23846,#23847,#23848,#23849,#23850,#23851,#23852,#23853,#23854,
#23855,#23856,#23857,#23858,#23859,#23860,#23861,#23862,#23863,#23864,#23865,
#23866,#23867,#23868,#23869,#23870,#23871,#23872,#23873,#23874,#23875,#23876,
#23877,#23878,#23879,#23880,#23881,#23882,#23883,#23884,#23885,#23886,#23887,
#23888,#23889,#23890,#23891,#23892,#23893,#23894,#23895,#23896,#23897,#23898,
#23899,#23900,#23901,#23902,#23903,#23904,#23905,#23906,#23907,#23908,#23909,
#23910,#23911,#23912,#23913,#23914,#23915,#23916,#23917,#23918,#23919,#23920,
#23921,#23922,#23923,#23924,#23925,#23926,#23927,#23928,#23929,#23930,#23931,
#23932,#23933,#23934,#23935,#23936,#23937,#23938,#23939,#23940,#23941,#23942,
#23943,#23944,#23945,#23946,#23947,#23948,#23949,#23950,#23951,#23952,#23953,
#23954,#23955,#23956,#23957,#23958,#23959,#23960,#23961,#23962,#23963,#23964),
 .UNSPECIFIED.,.F.,.F.,(4,2,2,2,2,2,2,2,2,2,2,2,2,2,2,2,2,2,2,2,2,2,2,2,
2,2,2,2,2,2,2,2,2,2,2,2,2,2,2,2,2,2,2,2,2,2,2,2,2,2,2,2,2,2,2,2,2,2,2,2,
2,2,2,2,2,2,2,2,2,2,2,2,2,2,2,2,2,2,2,2,2,2,2,2,2,2,2,2,2,2,2,2,2,2,2,4),
(-4.7594056615118,-4.75916330577551,-4.75479672118297,-4.75101129435165,
-4.74631039257129,-4.73891530401789,-4.70719446169042,-4.68232964832486,
-4.67415843637189,-4.66831673066041,-4.66558434060177,-4.66344945119886,
-4.66081785017293,-4.65550907898097,-4.61551129383112,-4.58934791442217,
-4.58149202619319,-4.57711419077999,-4.57332984680469,-4.56864428510768,
-4.55952917681014,-4.5179460685827,-4.49572971738074,-4.49033941106809,
-4.48769197418721,-4.48576971140616,-4.48316492434027,-4.47799320373326,
-4.4372816241478,-4.41151702480388,-4.40371457412652,-4.3993476243877,-4.39556225843814,
-4.3908619219216,-4.38346872551801,-4.35136889676871,-4.32679103395646,
-4.31866905695481,-4.31285339061202,-4.31012580084012,-4.30799108118059,
-4.30535524801632,-4.30002464936691,-4.26014378983,-4.23391405862721,-4.22604935253471,
-4.22166972820171,-4.21788555135072,-4.21320240403191,-4.20586823551696,
-4.17037682459832,-4.14826396719347,-4.13694184716023,-4.13345136577009,
-4.1312007176295,-4.12892069615413,-4.12529343302871,-4.11370198611476,
-4.07175374732255,-4.05264402967884,-4.04663861118359,-4.04264522344916,
-4.03878297021516,-4.03412481326402,-4.02272719228344,-3.98378700268498,
-3.96243294563211,-3.95713583172976,-3.95450653780041,-3.95258512661787,
-3.94996333437502,-3.94470465884547,-3.90444441227508,-3.87843060752874,
-3.87059482566671,-3.86622117402689,-3.86243658461173,-3.85774573179725,
-3.85038484489403,-3.81606518686078,-3.79311963822545,-3.78528875550116,
-3.77962833525715,-3.77692965610979,-3.77479566282334,-3.77213332398795,
-3.76666483697129,-3.74041889739658,-3.7152018259883,-3.69704299919251,
-3.69113025998066,-3.68715534970216,-3.68327872888863,-3.67856335764708,
-3.66680938922734,-3.6407755406643),.UNSPECIFIED.);
#1499=B_SPLINE_CURVE_WITH_KNOTS('',3,(#23969,#23970,#23971,#23972,#23973,
#23974,#23975,#23976,#23977,#23978,#23979,#23980,#23981,#23982,#23983,#23984,
#23985,#23986,#23987,#23988,#23989,#23990,#23991,#23992,#23993,#23994,#23995,
#23996,#23997,#23998,#23999,#24000,#24001,#24002,#24003,#24004,#24005,#24006,
#24007,#24008,#24009,#24010,#24011,#24012,#24013,#24014,#24015,#24016,#24017,
#24018,#24019,#24020,#24021,#24022,#24023,#24024,#24025,#24026,#24027,#24028,
#24029,#24030,#24031,#24032,#24033,#24034,#24035,#24036,#24037,#24038,#24039,
#24040,#24041,#24042,#24043,#24044,#24045,#24046,#24047,#24048,#24049,#24050,
#24051,#24052,#24053,#24054,#24055,#24056,#24057,#24058,#24059,#24060,#24061,
#24062,#24063,#24064,#24065,#24066,#24067,#24068,#24069,#24070,#24071,#24072,
#24073,#24074,#24075,#24076,#24077,#24078,#24079,#24080,#24081,#24082,#24083,
#24084,#24085,#24086,#24087,#24088,#24089,#24090,#24091,#24092,#24093,#24094,
#24095,#24096,#24097,#24098,#24099,#24100,#24101,#24102,#24103,#24104,#24105,
#24106,#24107,#24108,#24109,#24110,#24111,#24112,#24113,#24114,#24115,#24116,
#24117,#24118,#24119,#24120,#24121,#24122,#24123,#24124,#24125,#24126,#24127,
#24128,#24129,#24130,#24131,#24132,#24133,#24134,#24135,#24136,#24137,#24138,
#24139,#24140,#24141,#24142,#24143,#24144,#24145,#24146,#24147,#24148),
 .UNSPECIFIED.,.F.,.F.,(4,2,2,2,2,2,2,2,2,2,2,2,2,2,2,2,2,2,2,2,2,2,2,2,
2,2,2,2,2,2,2,2,2,2,2,2,2,2,2,2,2,2,2,2,2,2,2,2,2,2,2,2,2,2,2,2,2,2,2,2,
2,2,2,2,2,2,2,2,2,2,2,2,2,2,2,2,2,2,2,2,2,2,2,2,2,2,2,2,2,4),(-1.11906078687382,
-1.10181719756328,-1.07310984421461,-1.05985843780124,-1.05605785257306,
-1.05372509720322,-1.05147323486519,-1.04805226761362,-1.03757651050938,
-1.01829523112983,-0.978536216269192,-0.970740034232509,-0.966301768190049,
-0.962479250577419,-0.957762957824193,-0.9483293794914,-0.918682663292412,
-0.884394640018681,-0.879353917502312,-0.876727716162809,-0.874784802186414,
-0.872099751645558,-0.866597293280621,-0.843520949547377,-0.799894699950944,
-0.792492933571567,-0.788181185011461,-0.784343434533903,-0.779440633115032,
-0.768981750228283,-0.719754271889976,-0.704590573714031,-0.700636004371981,
-0.698269671638376,-0.696039532100416,-0.692729599962305,-0.683196969960408,
-0.666658254259388,-0.624802868658829,-0.616701865773417,-0.611773993293723,
-0.607933222527686,-0.603635240958969,-0.596301011987247,-0.561970404022273,
-0.528936071610351,-0.523812934010734,-0.521169299097288,-0.519227056119098,
-0.516560149568661,-0.511152813789114,-0.488987640439833,-0.447454108425651,
-0.438305665834496,-0.433584979099549,-0.429761832363847,-0.42532611326299,
-0.417324444703676,-0.390305014645148,-0.360961861247237,-0.348590528670158,
-0.344866857353913,-0.342550622966136,-0.340285453920716,-0.336800480941869,
-0.325739876617737,-0.304587218315611,-0.267819782241878,-0.260501620447879,
-0.255797549618092,-0.251975284101376,-0.247526455782177,-0.239460438723052,
-0.211942495746812,-0.18163303708696,-0.170569331621413,-0.166977681682724,
-0.164916385687827,-0.162677538410238,-0.159322775234664,-0.149421481335123,
-0.131848696431952,-0.0889657923829509,-0.0815460130446182,-0.0771890969075821,
-0.0737410664450437,-0.0690969878737329,-0.0600445857718003,-0.0481504936189692,
-9.99999999695689E-7),.UNSPECIFIED.);
#1500=B_SPLINE_CURVE_WITH_KNOTS('',3,(#24149,#24150,#24151,#24152,#24153,
#24154,#24155,#24156,#24157,#24158,#24159,#24160,#24161,#24162,#24163,#24164,
#24165,#24166,#24167,#24168,#24169,#24170,#24171,#24172,#24173,#24174,#24175,
#24176,#24177,#24178,#24179,#24180,#24181,#24182,#24183,#24184,#24185,#24186,
#24187,#24188,#24189,#24190,#24191,#24192,#24193,#24194,#24195,#24196,#24197,
#24198,#24199,#24200,#24201,#24202,#24203,#24204,#24205,#24206,#24207,#24208,
#24209,#24210,#24211,#24212,#24213,#24214,#24215,#24216,#24217,#24218,#24219,
#24220,#24221,#24222,#24223,#24224,#24225,#24226,#24227,#24228,#24229,#24230,
#24231,#24232,#24233,#24234,#24235,#24236,#24237,#24238,#24239,#24240,#24241,
#24242,#24243,#24244,#24245,#24246,#24247,#24248,#24249,#24250,#24251,#24252,
#24253,#24254,#24255,#24256,#24257,#24258,#24259,#24260,#24261,#24262,#24263,
#24264,#24265,#24266,#24267,#24268,#24269,#24270,#24271,#24272,#24273,#24274,
#24275,#24276,#24277,#24278,#24279,#24280,#24281,#24282,#24283,#24284,#24285,
#24286,#24287,#24288,#24289,#24290,#24291,#24292,#24293,#24294,#24295,#24296,
#24297,#24298,#24299,#24300,#24301,#24302,#24303,#24304,#24305,#24306,#24307,
#24308,#24309,#24310,#24311,#24312,#24313,#24314,#24315,#24316,#24317,#24318,
#24319,#24320,#24321,#24322,#24323,#24324,#24325,#24326,#24327,#24328,#24329,
#24330,#24331,#24332,#24333,#24334,#24335,#24336,#24337,#24338,#24339,#24340,
#24341,#24342),.UNSPECIFIED.,.F.,.F.,(4,2,2,2,2,2,2,2,2,2,2,2,2,2,2,2,2,
2,2,2,2,2,2,2,2,2,2,2,2,2,2,2,2,2,2,2,2,2,2,2,2,2,2,2,2,2,2,2,2,2,2,2,2,
2,2,2,2,2,2,2,2,2,2,2,2,2,2,2,2,2,2,2,2,2,2,2,2,2,2,2,2,2,2,2,2,2,2,2,2,
2,2,2,2,2,2,2,4),(-3.6407755406643,-3.62823903672922,-3.60700928379253,
-3.60172573997997,-3.59909903792633,-3.59717765690908,-3.59455315925463,
-3.58928091310584,-3.54908947617732,-3.52303528128578,-3.51519394260481,
-3.51081905962426,-3.50703443352383,-3.50234486406071,-3.4929005906048,
-3.45156694260271,-3.42942943882715,-3.42404749039955,-3.42140165389513,
-3.41947945289459,-3.41687313615243,-3.41169372364897,-3.37102076726245,
-3.35234718742111,-3.34381987960854,-3.33679933930009,-3.3325947975643,
-3.32878302319415,-3.32389942684178,-3.31307527719816,-3.27326274865875,
-3.25161763985724,-3.24628853709875,-3.24365289391343,-3.24173109409809,
-3.23911501905084,-3.23388618372287,-3.19346535835553,-3.16753769189963,
-3.15971312550493,-3.15534155112109,-3.15155645389728,-3.14686198986802,
-3.13948935050053,-3.1057489287751,-3.08238121793475,-3.07070644041987,
-3.06718040000695,-3.06492211178239,-3.06292211275666,-3.05958180117751,
-3.05037771374336,-3.01440216970852,-2.99645323504766,-2.98433891606545,
-2.97919187937283,-2.97535497670775,-2.97123095057607,-2.96459447602382,
-2.93872912865183,-2.93340985404414,-2.90132098855327,-2.89249856975364,
-2.88921095074664,-2.88702328263193,-2.88469439189205,-2.88084226481917,
-2.8651484840993,-2.81840307593977,-2.80672333963632,-2.80204735075143,
-2.79818063723277,-2.79419315902494,-2.78821736028043,-2.76942161240239,
-2.7294038732124,-2.71583954369029,-2.7120227562128,-2.70970158445304,-2.70748275509494,
-2.70414770152325,-2.69423857097695,-2.67658905883789,-2.63377780420986,
-2.62637505797203,-2.62204939522561,-2.61829579818965,-2.6135555260694,
-2.60383795248285,-2.57737223856036,-2.54430079730469,-2.53664274838501,
-2.53352848575528,-2.53135035542992,-2.52895156704685,-2.52477599256707,
-2.52207415166318),.UNSPECIFIED.);
#1501=B_SPLINE_CURVE_WITH_KNOTS('',3,(#24347,#24348,#24349,#24350,#24351,
#24352,#24353,#24354,#24355,#24356,#24357,#24358,#24359,#24360,#24361,#24362,
#24363,#24364,#24365,#24366,#24367,#24368,#24369,#24370,#24371,#24372,#24373,
#24374,#24375,#24376,#24377,#24378,#24379,#24380,#24381,#24382,#24383,#24384,
#24385,#24386,#24387,#24388,#24389,#24390,#24391,#24392,#24393,#24394,#24395,
#24396,#24397,#24398,#24399,#24400,#24401,#24402,#24403,#24404,#24405,#24406,
#24407,#24408,#24409,#24410,#24411,#24412,#24413,#24414,#24415,#24416,#24417,
#24418,#24419,#24420,#24421,#24422,#24423,#24424,#24425,#24426,#24427,#24428,
#24429,#24430,#24431,#24432,#24433,#24434,#24435,#24436,#24437,#24438,#24439,
#24440,#24441,#24442,#24443,#24444,#24445,#24446,#24447,#24448,#24449,#24450,
#24451,#24452,#24453,#24454,#24455,#24456,#24457,#24458,#24459,#24460,#24461,
#24462,#24463,#24464,#24465,#24466,#24467,#24468,#24469,#24470,#24471,#24472,
#24473,#24474,#24475,#24476,#24477,#24478,#24479,#24480,#24481,#24482,#24483,
#24484,#24485,#24486,#24487,#24488,#24489,#24490,#24491,#24492,#24493,#24494,
#24495,#24496,#24497,#24498,#24499,#24500,#24501,#24502,#24503,#24504,#24505,
#24506,#24507,#24508,#24509,#24510,#24511,#24512,#24513,#24514,#24515,#24516,
#24517,#24518,#24519,#24520,#24521,#24522,#24523,#24524,#24525,#24526,#24527,
#24528,#24529,#24530,#24531,#24532,#24533,#24534,#24535,#24536,#24537,#24538,
#24539,#24540,#24541,#24542,#24543,#24544,#24545,#24546),.UNSPECIFIED.,
 .F.,.F.,(4,2,2,2,2,2,2,2,2,2,2,2,2,2,2,2,2,2,2,2,2,2,2,2,2,2,2,2,2,2,2,
2,2,2,2,2,2,2,2,2,2,2,2,2,2,2,2,2,2,2,2,2,2,2,2,2,2,2,2,2,2,2,2,2,2,2,2,
2,2,2,2,2,2,2,2,2,2,2,2,2,2,2,2,2,2,2,2,2,2,2,2,2,2,2,2,2,2,2,2,4),(-2.23776655190534,
-2.22778578623218,-2.21664579712278,-2.21168012354498,-2.20782513931058,
-2.20359282740332,-2.19657021046483,-2.1880595607134,-2.16951684413861,
-2.12944471222924,-2.12375041193938,-2.1210291076989,-2.11887273919109,
-2.11617347515858,-2.11059588467045,-2.10293885699918,-2.08100606667912,
-2.04538751067939,-2.03803063366754,-2.03331568678251,-2.02949337242211,
-2.02505434611152,-2.01703446455939,-1.98986969167966,-1.96024391688906,
-1.94827036633159,-1.94458385716107,-1.94227588363341,-1.94000430311049,
-1.9364876183063,-1.92511940665894,-1.90291729705943,-1.86768145878101,
-1.86031451822166,-1.85559661619329,-1.85177409368628,-1.84733727421533,
-1.83932839729022,-1.81224894927909,-1.78278746473526,-1.77058686454044,
-1.76687912336045,-1.76456653678717,-1.76229886971181,-1.75880094410284,
-1.74761424893408,-1.7260357946128,-1.68990457598868,-1.68256316367106,
-1.67785265847939,-1.67403051214529,-1.66958782970314,-1.66155027080362,
-1.63424936346443,-1.60436186620528,-1.59274498114508,-1.58909299526128,
-1.58679245191756,-1.58451411436486,-1.58096560717457,-1.56928261965791,
-1.54595979798705,-1.51228753497942,-1.5048880403939,-1.50016062331006,
-1.4963374611204,-1.49190778691123,-1.48393431199371,-1.45712731518792,
-1.42819116049543,-1.41525896850161,-1.41148607262065,-1.40915932826513,
-1.40690296117056,-1.40345985565169,-1.39278493394391,-1.37288208127055,
-1.33416753650424,-1.32627293824911,-1.32181350710689,-1.31799236189653,
-1.3133026310134,-1.30400972084381,-1.29168642256704,-1.26662142927137,
-1.24049651601774,-1.23500310922807,-1.23231986406611,-1.23016320455181,
-1.22742495387376,-1.22164013264208,-1.21359765320601,-1.18957061295041,
-1.15685959066571,-1.14944581247,-1.14471424361301,-1.14089081936404,-1.13646428735957,
-1.12850626248216,-1.11906078687382),.UNSPECIFIED.);
#1502=B_SPLINE_CURVE_WITH_KNOTS('',3,(#24547,#24548,#24549,#24550,#24551,
#24552,#24553,#24554,#24555,#24556,#24557,#24558,#24559,#24560,#24561,#24562,
#24563,#24564,#24565,#24566,#24567,#24568,#24569,#24570,#24571,#24572,#24573,
#24574,#24575,#24576,#24577,#24578,#24579,#24580,#24581,#24582,#24583,#24584,
#24585,#24586,#24587,#24588,#24589,#24590,#24591,#24592,#24593,#24594,#24595,
#24596,#24597,#24598,#24599,#24600,#24601,#24602,#24603,#24604,#24605,#24606,
#24607,#24608,#24609,#24610,#24611,#24612,#24613,#24614,#24615,#24616,#24617,
#24618,#24619,#24620,#24621,#24622,#24623,#24624,#24625,#24626,#24627,#24628,
#24629,#24630,#24631,#24632,#24633,#24634,#24635,#24636,#24637,#24638,#24639,
#24640,#24641,#24642,#24643,#24644,#24645,#24646,#24647,#24648,#24649,#24650,
#24651,#24652,#24653,#24654,#24655,#24656,#24657,#24658,#24659,#24660,#24661,
#24662,#24663,#24664,#24665,#24666,#24667,#24668,#24669,#24670,#24671,#24672,
#24673,#24674,#24675,#24676,#24677,#24678,#24679,#24680,#24681,#24682,#24683,
#24684,#24685,#24686,#24687,#24688,#24689,#24690,#24691,#24692,#24693,#24694,
#24695,#24696,#24697,#24698,#24699,#24700,#24701,#24702,#24703,#24704,#24705,
#24706,#24707,#24708,#24709,#24710,#24711,#24712,#24713,#24714,#24715,#24716,
#24717,#24718,#24719,#24720,#24721,#24722,#24723,#24724,#24725,#24726,#24727,
#24728),.UNSPECIFIED.,.F.,.F.,(4,2,2,2,2,2,2,2,2,2,2,2,2,2,2,2,2,2,2,2,
2,2,2,2,2,2,2,2,2,2,2,2,2,2,2,2,2,2,2,2,2,2,2,2,2,2,2,2,2,2,2,2,2,2,2,2,
2,2,2,2,2,2,2,2,2,2,2,2,2,2,2,2,2,2,2,2,2,2,2,2,2,2,2,2,2,2,2,2,2,2,4),
(-2.52207415166318,-2.50206841203732,-2.46446175317106,-2.45172959676644,
-2.44635922366383,-2.44252463193816,-2.43848787273917,-2.43227004783753,
-2.41069345718137,-2.3885425896863,-2.36325986778271,-2.35778913772044,
-2.35512636640086,-2.35299237400426,-2.35029414092764,-2.34463609308825,
-2.33681053428452,-2.31388984004935,-2.27957568644593,-2.27221660022988,
-2.26752623532568,-2.26374165393042,-2.2593675818048,-2.25152992085083,
-2.22550200042049,-2.18521970032241,-2.17995933267413,-2.17733713184624,
-2.17541562739576,-2.17278648651977,-2.16749056544787,-2.14614859757975,
-2.10723329517739,-2.0958338754606,-2.09117530941448,-2.08731277540526,
-2.08331918032209,-2.07731364598697,-2.05820821299268,-2.0163187509785,
-2.00463549312324,-2.0009988307737,-1.99871665196085,-1.99646751707909,
-1.99298496162698,-1.9817412005249,-1.95989985959076,-1.92405458162906,
-1.9167314612759,-1.91205125203168,-1.90826690519131,-1.90388424971708,
-1.89600615329143,-1.86967868930399,-1.82991359984729,-1.82455454730925,
-1.82191297490756,-1.81977812844573,-1.81705613250725,-1.81127200173337,
-1.80321084471109,-1.77898103129641,-1.74644665056317,-1.73905782061798,
-1.7343583600182,-1.73057254762485,-1.72620380801291,-1.71839467068711,
-1.6925848514777,-1.65189557172077,-1.64671162497265,-1.6441041290424,-1.64218160476008,
-1.63953604339504,-1.63415702417674,-1.61205188560703,-1.57080945029454,
-1.56129886500964,-1.55659637503463,-1.55281023028015,-1.54844343437122,
-1.54064428709557,-1.51490962759984,-1.47408083978773,-1.46892385649621,
-1.46632162108433,-1.4643987424934,-1.46174729928031,-1.45633810353154,
-1.43394943723756,-1.40333270505807),.UNSPECIFIED.);
#1503=B_SPLINE_CURVE_WITH_KNOTS('',3,(#24733,#24734,#24735,#24736,#24737,
#24738,#24739,#24740,#24741,#24742,#24743,#24744,#24745,#24746,#24747,#24748,
#24749,#24750,#24751,#24752,#24753,#24754,#24755,#24756,#24757,#24758,#24759,
#24760,#24761,#24762,#24763,#24764,#24765,#24766,#24767,#24768,#24769,#24770,
#24771,#24772,#24773,#24774,#24775,#24776,#24777,#24778,#24779,#24780,#24781,
#24782,#24783,#24784,#24785,#24786,#24787,#24788,#24789,#24790,#24791,#24792,
#24793,#24794,#24795,#24796,#24797,#24798,#24799,#24800,#24801,#24802,#24803,
#24804,#24805,#24806,#24807,#24808,#24809,#24810,#24811,#24812,#24813,#24814,
#24815,#24816,#24817,#24818,#24819,#24820,#24821,#24822,#24823,#24824,#24825,
#24826,#24827,#24828,#24829,#24830,#24831,#24832,#24833,#24834,#24835,#24836,
#24837,#24838,#24839,#24840,#24841,#24842,#24843,#24844,#24845,#24846,#24847,
#24848,#24849,#24850,#24851,#24852,#24853,#24854,#24855,#24856,#24857,#24858,
#24859,#24860,#24861,#24862,#24863,#24864,#24865,#24866,#24867,#24868,#24869,
#24870,#24871,#24872,#24873,#24874,#24875,#24876,#24877,#24878,#24879,#24880,
#24881,#24882,#24883,#24884,#24885,#24886,#24887,#24888,#24889,#24890,#24891,
#24892,#24893,#24894,#24895,#24896,#24897,#24898,#24899,#24900,#24901,#24902,
#24903,#24904,#24905,#24906,#24907,#24908,#24909,#24910,#24911,#24912,#24913,
#24914,#24915,#24916),.UNSPECIFIED.,.F.,.F.,(4,2,2,2,2,2,2,2,2,2,2,2,2,
2,2,2,2,2,2,2,2,2,2,2,2,2,2,2,2,2,2,2,2,2,2,2,2,2,2,2,2,2,2,2,2,2,2,2,2,
2,2,2,2,2,2,2,2,2,2,2,2,2,2,2,2,2,2,2,2,2,2,2,2,2,2,2,2,2,2,2,2,2,2,2,2,
2,2,2,2,2,2,4),(-3.35656936323946,-3.35555127465481,-3.32125403551656,-3.28820983530958,
-3.28081612012118,-3.27650623210897,-3.27266845797338,-3.26776330812124,
-3.25974149257815,-3.21776520366904,-3.19545770585155,-3.1900357074741,
-3.18736623355975,-3.18542419206659,-3.18278384966788,-3.17767527426617,
-3.14438515086975,-3.11390942837666,-3.10446815054549,-3.09975052997067,
-3.09592804175039,-3.09149104512586,-3.0837004338175,-3.04385229748872,
-3.024599256753,-3.0141329395229,-3.01071300288342,-3.00846140166676,-3.00612842555101,
-3.0023267254962,-2.98906039023524,-2.96038806981269,-2.93372108698596,
-2.92576600805621,-2.92134013310743,-2.91751671201493,-2.91278442265208,
-2.90536798090327,-2.87272536694968,-2.84861875839361,-2.84056139604117,
-2.83476916045929,-2.83202954047909,-2.8298728733851,-2.82719094453908,
-2.82170433253122,-2.79694262892508,-2.75551924072584,-2.74791231423617,
-2.74351509727161,-2.73968923629371,-2.73491848454737,-2.72519181982528,
-2.69923303146447,-2.66701656038511,-2.65836964724076,-2.65508520061442,
-2.65288217854081,-2.65051509482237,-2.64655600455908,-2.62952967427972,
-2.606724886456,-2.5761167337456,-2.56932854922896,-2.56514525967573,-2.56127491228829,
-2.55611414860776,-2.54410822702096,-2.52643877688118,-2.49218433746845,
-2.48127201763248,-2.47769798563009,-2.47564030585883,-2.47339885108536,
-2.47002962529166,-2.4600033876834,-2.44206790014104,-2.39988659582721,
-2.3923755358656,-2.38799913327179,-2.38420743676287,-2.37942535194345,
-2.36963725670147,-2.34279343300518,-2.30884761957336,-2.30220229640161,
-2.29951233806927,-2.29732480005187,-2.29492679668286,-2.29082494000496,
-2.27093300085587,-2.23776655190534),.UNSPECIFIED.);
#1504=B_SPLINE_CURVE_WITH_KNOTS('',3,(#24917,#24918,#24919,#24920,#24921,
#24922,#24923,#24924,#24925,#24926,#24927,#24928,#24929,#24930,#24931,#24932,
#24933,#24934,#24935,#24936,#24937,#24938,#24939,#24940,#24941,#24942,#24943,
#24944,#24945,#24946,#24947,#24948,#24949,#24950,#24951,#24952,#24953,#24954,
#24955,#24956,#24957,#24958,#24959,#24960,#24961,#24962,#24963,#24964,#24965,
#24966,#24967,#24968,#24969,#24970,#24971,#24972,#24973,#24974,#24975,#24976,
#24977,#24978,#24979,#24980,#24981,#24982,#24983,#24984,#24985,#24986,#24987,
#24988,#24989,#24990,#24991,#24992,#24993,#24994,#24995,#24996,#24997,#24998,
#24999,#25000,#25001,#25002,#25003,#25004,#25005,#25006,#25007,#25008,#25009,
#25010,#25011,#25012,#25013,#25014,#25015,#25016,#25017,#25018,#25019,#25020,
#25021,#25022,#25023,#25024,#25025,#25026,#25027,#25028,#25029,#25030,#25031,
#25032,#25033,#25034,#25035,#25036,#25037,#25038,#25039,#25040,#25041,#25042,
#25043,#25044,#25045,#25046,#25047,#25048,#25049,#25050,#25051,#25052,#25053,
#25054,#25055,#25056,#25057,#25058,#25059,#25060,#25061,#25062,#25063,#25064,
#25065,#25066,#25067,#25068,#25069,#25070,#25071,#25072,#25073,#25074,#25075,
#25076,#25077,#25078,#25079,#25080,#25081,#25082,#25083,#25084,#25085,#25086,
#25087,#25088,#25089,#25090,#25091,#25092,#25093,#25094,#25095,#25096,#25097,
#25098,#25099,#25100,#25101,#25102,#25103,#25104,#25105,#25106,#25107,#25108,
#25109,#25110,#25111,#25112),.UNSPECIFIED.,.F.,.F.,(4,2,2,2,2,2,2,2,2,2,
2,2,2,2,2,2,2,2,2,2,2,2,2,2,2,2,2,2,2,2,2,2,2,2,2,2,2,2,2,2,2,2,2,2,2,2,
2,2,2,2,2,2,2,2,2,2,2,2,2,2,2,2,2,2,2,2,2,2,2,2,2,2,2,2,2,2,2,2,2,2,2,2,
2,2,2,2,2,2,2,2,2,2,2,2,2,2,2,4),(-1.40333270505807,-1.39180496678422,-1.38392532244935,
-1.37908510902709,-1.37528713446274,-1.37101173818054,-1.36365501010383,
-1.35459247470321,-1.33394975120503,-1.30206072713359,-1.2929855579044,
-1.28966239596659,-1.2876652123249,-1.28540198829625,-1.28185430165187,
-1.26996114954773,-1.24578375012125,-1.21317340681559,-1.20578470752908,
-1.20108506819908,-1.19729894975835,-1.19292967789213,-1.18511908715568,
-1.1593012102664,-1.11861909634247,-1.11343263107251,-1.1108245046547,-1.10890183810593,
-1.10625649130622,-1.10087928630155,-1.07879355873006,-1.03761450685677,
-1.02804453512103,-1.02333075030235,-1.0195435390437,-1.01518434310488,
-1.00742336881242,-0.981972349650676,-0.942889925412528,-0.936347579360866,
-0.933521154772953,-0.931375470272141,-0.928851084358466,-0.924080862653826,
-0.917843806981941,-0.902339974435919,-0.864568329010454,-0.852002180895898,
-0.846648034177631,-0.842815239216356,-0.838771758290313,-0.83252560572496,
-0.810600085930862,-0.777169269684361,-0.761045995716779,-0.757048841356857,
-0.754688083131964,-0.752491564931561,-0.749275647617909,-0.740329476473356,
-0.725306406312121,-0.689299238443309,-0.674905702836174,-0.669275744450861,
-0.665746532577764,-0.661838468612679,-0.656277745601053,-0.641234339962453,
-0.615943597650611,-0.585574514865633,-0.58023773391861,-0.577600153769365,
-0.575464728532464,-0.572737155145714,-0.566924620767498,-0.558810478590108,
-0.534280246766163,-0.502134147682818,-0.494740521236823,-0.490039151188441,
-0.486252506650955,-0.481883586689752,-0.474076312195854,-0.448286801894074,
-0.407543046084399,-0.402367119870654,-0.39976088305286,-0.397837877267002,
-0.3951898587088,-0.389799803486504,-0.367596725965957,-0.326050794354874,
-0.316907653683928,-0.312215329333407,-0.308429144525465,-0.304053194457995,
-0.296212098783039,-0.284404947939953),.UNSPECIFIED.);
#1505=B_SPLINE_CURVE_WITH_KNOTS('',3,(#25117,#25118,#25119,#25120,#25121,
#25122,#25123,#25124,#25125,#25126,#25127,#25128,#25129,#25130,#25131,#25132,
#25133,#25134,#25135,#25136,#25137,#25138,#25139,#25140,#25141,#25142,#25143,
#25144,#25145,#25146,#25147,#25148,#25149,#25150,#25151,#25152,#25153,#25154,
#25155,#25156,#25157,#25158,#25159,#25160,#25161,#25162,#25163,#25164,#25165,
#25166,#25167,#25168,#25169,#25170,#25171,#25172,#25173,#25174,#25175,#25176,
#25177,#25178,#25179,#25180,#25181,#25182,#25183,#25184,#25185,#25186,#25187,
#25188,#25189,#25190,#25191,#25192,#25193,#25194,#25195,#25196,#25197,#25198,
#25199,#25200,#25201,#25202,#25203,#25204,#25205,#25206,#25207,#25208,#25209,
#25210,#25211,#25212,#25213,#25214,#25215,#25216,#25217,#25218,#25219,#25220,
#25221,#25222,#25223,#25224,#25225,#25226,#25227,#25228,#25229,#25230,#25231,
#25232,#25233,#25234,#25235,#25236,#25237,#25238,#25239,#25240,#25241,#25242,
#25243,#25244,#25245,#25246,#25247,#25248,#25249,#25250,#25251,#25252,#25253,
#25254,#25255,#25256,#25257,#25258,#25259,#25260,#25261,#25262,#25263,#25264,
#25265,#25266,#25267,#25268,#25269,#25270,#25271,#25272,#25273,#25274,#25275,
#25276,#25277,#25278,#25279,#25280,#25281,#25282,#25283,#25284,#25285,#25286,
#25287,#25288,#25289,#25290,#25291,#25292,#25293,#25294,#25295,#25296,#25297,
#25298,#25299,#25300,#25301,#25302,#25303,#25304,#25305,#25306,#25307,#25308),
 .UNSPECIFIED.,.F.,.F.,(4,2,2,2,2,2,2,2,2,2,2,2,2,2,2,2,2,2,2,2,2,2,2,2,
2,2,2,2,2,2,2,2,2,2,2,2,2,2,2,2,2,2,2,2,2,2,2,2,2,2,2,2,2,2,2,2,2,2,2,2,
2,2,2,2,2,2,2,2,2,2,2,2,2,2,2,2,2,2,2,2,2,2,2,2,2,2,2,2,2,2,2,2,2,2,2,4),
(-4.47541535506956,-4.46168686137262,-4.44533441280584,-4.43587076265126,
-4.43256971887689,-4.43034159877718,-4.42797315272518,-4.42400722012639,
-4.40863814634345,-4.35957448054162,-4.34919030325548,-4.3443013728649,
-4.3404657866815,-4.33614740160655,-4.32871089717986,-4.28530688791141,
-4.26206648242813,-4.25654768593994,-4.25385985597878,-4.25191710041922,
-4.24929425656539,-4.24426872711686,-4.20985718613612,-4.18035113457065,
-4.17092206770026,-4.16620681143604,-4.16238453193918,-4.15794585879716,
-4.15014716487225,-4.11038765894985,-4.09108798791207,-4.08060676665653,
-4.07718518013403,-4.07493325664548,-4.0726008339112,-4.06880135011771,
-4.05555828463033,-4.02687172384334,-4.00019836087532,-3.9922427238327,
-3.98781690381526,-3.98399372975824,-3.97926200361188,-3.97184697266457,
-3.9391156034799,-3.91507687253339,-3.90703168782298,-3.90124602681201,
-3.89850774136233,-3.89635124901468,-3.89366845105915,-3.88817669969464,
-3.86208059548485,-3.83705228453644,-3.82471930302464,-3.81542028956979,
-3.81072961079175,-3.80690864128574,-3.80245048847723,-3.79456111958678,
-3.75575123577177,-3.73588263896161,-3.72521886941121,-3.72177702776948,
-3.71952101947594,-3.71747823061421,-3.71398209636885,-3.70372433307347,
-3.67282322957182,-3.64501249227021,-3.63690987293162,-3.63245405580393,
-3.62863283941965,-3.62393900825083,-3.61492168625518,-3.5732146648061,
-3.5567089770894,-3.54718924110773,-3.54388110561216,-3.54165151987289,
-3.53928502288142,-3.53532886607847,-3.520127671446,-3.47095822590636,-3.46051875941119,
-3.45561973619867,-3.45178272220362,-3.44746948386088,-3.44005925236906,
-3.39646855509076,-3.37334785738748,-3.36784106763373,-3.36515533871445,
-3.36321256861206,-3.36058746060944,-3.35656936323946),.UNSPECIFIED.);
#1506=B_SPLINE_CURVE_WITH_KNOTS('',3,(#25310,#25311,#25312,#25313,#25314,
#25315,#25316,#25317,#25318,#25319,#25320,#25321,#25322,#25323,#25324,#25325,
#25326,#25327,#25328,#25329,#25330,#25331,#25332,#25333,#25334,#25335,#25336,
#25337,#25338,#25339,#25340,#25341,#25342,#25343,#25344,#25345,#25346,#25347,
#25348,#25349,#25350,#25351,#25352,#25353,#25354,#25355,#25356,#25357,#25358,
#25359,#25360,#25361,#25362,#25363),.UNSPECIFIED.,.F.,.F.,(4,2,2,2,2,2,
2,2,2,2,2,2,2,2,2,2,2,2,2,2,2,2,2,2,2,2,4),(-0.284404947939953,-0.270172367198298,
-0.229874565476045,-0.224611707048033,-0.22198834889193,-0.220066038374403,
-0.217435847933057,-0.212137987545278,-0.190789670724902,-0.151863692286156,
-0.140453460071792,-0.135791956829375,-0.131927557084387,-0.12793261428107,
-0.127722266749346,-0.127515952580895,-0.127311165663978,-0.120991416525271,
-0.0984562989763039,-0.068449773798942,-0.0501364229208393,-0.0460294130521238,
-0.0436447259434375,-0.0414592423917343,-0.0383062002011589,-0.0346567302149804,
-1.00000007596801E-6),.UNSPECIFIED.);
#1507=B_SPLINE_CURVE_WITH_KNOTS('',3,(#25364,#25365,#25366,#25367,#25368,
#25369,#25370,#25371,#25372,#25373,#25374,#25375,#25376,#25377,#25378,#25379,
#25380,#25381,#25382,#25383,#25384,#25385,#25386,#25387,#25388,#25389,#25390,
#25391,#25392,#25393,#25394,#25395,#25396,#25397,#25398,#25399,#25400,#25401,
#25402,#25403,#25404,#25405,#25406,#25407,#25408,#25409,#25410,#25411,#25412,
#25413,#25414,#25415,#25416,#25417,#25418,#25419,#25420,#25421,#25422,#25423,
#25424,#25425,#25426,#25427,#25428,#25429,#25430,#25431,#25432,#25433,#25434,
#25435,#25436,#25437,#25438,#25439,#25440,#25441,#25442,#25443,#25444,#25445,
#25446,#25447,#25448,#25449,#25450,#25451,#25452,#25453,#25454,#25455,#25456,
#25457,#25458,#25459,#25460,#25461,#25462,#25463,#25464,#25465,#25466,#25467,
#25468,#25469,#25470,#25471,#25472,#25473,#25474,#25475,#25476,#25477,#25478,
#25479,#25480,#25481,#25482,#25483,#25484,#25485,#25486,#25487,#25488,#25489,
#25490,#25491,#25492,#25493,#25494,#25495,#25496,#25497,#25498,#25499,#25500,
#25501,#25502,#25503),.UNSPECIFIED.,.F.,.F.,(4,2,2,2,2,2,2,2,2,2,2,2,2,
2,2,2,2,2,2,2,2,2,2,2,2,2,2,2,2,2,2,2,2,2,2,2,2,2,2,2,2,2,2,2,2,2,2,2,2,
2,2,2,2,2,2,2,2,2,2,2,2,2,2,2,2,2,2,2,2,4),(-2.78528382917142,-2.75364564113469,
-2.7479236220945,-2.74389220912167,-2.73990123562933,-2.73603756310898,
-2.730500203602,-2.71674562910167,-2.68539492617632,-2.66658365863005,-2.65633953007895,
-2.65293211477355,-2.6506989187282,-2.64839843243281,-2.64467601346079,
-2.63205701367805,-2.60292403279826,-2.57596910413347,-2.5680093946514,
-2.56361064585203,-2.55982826922107,-2.55517076527411,-2.54619342395583,
-2.50445187477274,-2.4821865743147,-2.47679137541237,-2.47414315349886,
-2.47222103006302,-2.4696174720036,-2.46445118591793,-2.42371839248954,
-2.39797007301252,-2.39017024092275,-2.38580409826865,-2.38201906787512,
-2.37731867580989,-2.3699244246843,-2.33819048119904,-2.3133407563055,-2.30517252526879,
-2.29933255121657,-2.29660064970405,-2.29446597990667,-2.29183444493081,
-2.28652522000183,-2.25581462821527,-2.23078124691386,-2.21582959706935,
-2.2102821720436,-2.20637775030518,-2.2028480572464,-2.19810938354337,-2.18620812017513,
-2.14779364809033,-2.12661720906565,-2.12133974114435,-2.11871432878208,
-2.11679312333415,-2.11416773570442,-2.10889029317753,-2.07714911463725,
-2.04501048191141,-2.03575757397118,-2.03110424504657,-2.02732192769614,
-2.02291949771949,-2.01516199718309,-1.97526101342384,-1.95598866852601,
-1.95100679492342),.UNSPECIFIED.);
#1508=B_SPLINE_CURVE_WITH_KNOTS('',3,(#25508,#25509,#25510,#25511,#25512,
#25513,#25514,#25515,#25516,#25517,#25518,#25519,#25520,#25521,#25522,#25523,
#25524,#25525,#25526,#25527,#25528,#25529,#25530,#25531,#25532,#25533,#25534,
#25535,#25536,#25537,#25538,#25539,#25540,#25541,#25542,#25543,#25544,#25545,
#25546,#25547,#25548,#25549,#25550,#25551,#25552,#25553,#25554,#25555,#25556,
#25557,#25558,#25559,#25560,#25561,#25562,#25563,#25564,#25565,#25566,#25567,
#25568,#25569,#25570,#25571,#25572,#25573,#25574,#25575,#25576,#25577,#25578,
#25579,#25580,#25581,#25582,#25583,#25584,#25585,#25586,#25587,#25588,#25589,
#25590,#25591,#25592,#25593,#25594,#25595,#25596,#25597,#25598,#25599,#25600,
#25601,#25602,#25603,#25604,#25605,#25606,#25607,#25608,#25609,#25610,#25611,
#25612,#25613,#25614,#25615,#25616,#25617,#25618,#25619,#25620,#25621,#25622,
#25623,#25624,#25625,#25626,#25627,#25628,#25629,#25630,#25631,#25632,#25633,
#25634,#25635,#25636,#25637,#25638,#25639,#25640,#25641,#25642,#25643,#25644,
#25645,#25646,#25647,#25648,#25649,#25650,#25651,#25652,#25653,#25654,#25655,
#25656,#25657,#25658,#25659,#25660,#25661,#25662,#25663,#25664,#25665,#25666,
#25667,#25668,#25669,#25670,#25671,#25672,#25673,#25674,#25675,#25676,#25677,
#25678,#25679,#25680,#25681,#25682,#25683,#25684,#25685,#25686,#25687,#25688,
#25689,#25690,#25691,#25692,#25693,#25694,#25695,#25696,#25697),
 .UNSPECIFIED.,.F.,.F.,(4,2,2,2,2,2,2,2,2,2,2,2,2,2,2,2,2,2,2,2,2,2,2,2,
2,2,2,2,2,2,2,2,2,2,2,2,2,2,2,2,2,2,2,2,2,2,2,2,2,2,2,2,2,2,2,2,2,2,2,2,
2,2,2,2,2,2,2,2,2,2,2,2,2,2,2,2,2,2,2,2,2,2,2,2,2,2,2,2,2,2,2,2,2,2,4),
(-5.59412685259837,-5.59079749322766,-5.58706650607828,-5.58325343288845,
-5.57816116599502,-5.56703780700355,-5.55515778378523,-5.52852241784322,
-5.50624596204639,-5.50081915829663,-5.49814446445037,-5.49620376172452,
-5.49357538154047,-5.48832539662164,-5.44800403895801,-5.42206233474434,
-5.41422411608657,-5.40983907550084,-5.40603862202533,-5.40131995821258,
-5.39389820250337,-5.36222593143895,-5.33716186302814,-5.32894506223185,
-5.32307482262384,-5.32033251940357,-5.31818374485663,-5.31552536636805,
-5.31016011256005,-5.28001907319866,-5.26691352921521,-5.24678523095788,
-5.2372719210887,-5.23253588769219,-5.22870608381427,-5.22426871236286,
-5.2164973218407,-5.17337899731163,-5.15076202123844,-5.1453029460488,-5.1426215065187,
-5.14067493464708,-5.13803367491682,-5.13292813033915,-5.09216515141719,
-5.07358446581026,-5.06116526850781,-5.05593904557034,-5.05205763222523,
-5.04789803646789,-5.04122847992687,-5.01557096191177,-4.98367582600429,
-4.97444231866549,-4.96804160561886,-4.96519274997924,-4.96303123623948,
-4.96044185452032,-4.95556893832469,-4.91973687145443,-4.89137995357993,
-4.88196568341991,-4.87725561231467,-4.87343668509704,-4.8690010824479,
-4.86120608588939,-4.82140137807094,-4.79333583803964,-4.78903001248988,
-4.7865895642039,-4.78439568255832,-4.78128742872615,-4.77381971697473,
-4.73603092395748,-4.71084072008013,-4.70308375071154,-4.69869793736525,
-4.69486983733739,-4.69008022840632,-4.682466772192,-4.63995977772311,-4.61749354531017,
-4.61205413732695,-4.60938064304101,-4.60743790905339,-4.60479978098107,
-4.59953957600136,-4.55924132226508,-4.53329226432026,-4.52543286037423,
-4.52102660453907,-4.51720154419937,-4.51244309002777,-4.50278325045138,
-4.47541535506956),.UNSPECIFIED.);
#1509=B_SPLINE_CURVE_WITH_KNOTS('',3,(#25698,#25699,#25700,#25701,#25702,
#25703,#25704,#25705,#25706,#25707,#25708,#25709,#25710,#25711,#25712,#25713,
#25714,#25715,#25716,#25717,#25718,#25719,#25720,#25721,#25722,#25723,#25724,
#25725,#25726,#25727,#25728,#25729,#25730,#25731,#25732,#25733,#25734,#25735,
#25736,#25737,#25738,#25739,#25740,#25741,#25742,#25743,#25744,#25745,#25746,
#25747,#25748,#25749,#25750,#25751,#25752,#25753,#25754,#25755,#25756,#25757,
#25758,#25759,#25760,#25761,#25762,#25763,#25764,#25765,#25766,#25767,#25768,
#25769,#25770,#25771,#25772,#25773,#25774,#25775,#25776,#25777,#25778,#25779,
#25780,#25781,#25782,#25783,#25784,#25785,#25786,#25787,#25788,#25789,#25790,
#25791,#25792,#25793,#25794,#25795,#25796,#25797,#25798,#25799,#25800,#25801,
#25802,#25803,#25804,#25805,#25806,#25807,#25808,#25809,#25810,#25811,#25812,
#25813,#25814,#25815,#25816,#25817,#25818,#25819,#25820,#25821,#25822,#25823,
#25824,#25825,#25826,#25827,#25828,#25829,#25830,#25831,#25832,#25833,#25834,
#25835,#25836,#25837,#25838,#25839,#25840,#25841,#25842,#25843,#25844,#25845,
#25846,#25847,#25848,#25849,#25850,#25851,#25852,#25853,#25854,#25855,#25856,
#25857,#25858,#25859,#25860,#25861,#25862,#25863,#25864,#25865,#25866,#25867,
#25868,#25869,#25870,#25871,#25872,#25873,#25874,#25875,#25876,#25877,#25878,
#25879,#25880,#25881,#25882,#25883,#25884,#25885,#25886,#25887,#25888,#25889,
#25890,#25891),.UNSPECIFIED.,.F.,.F.,(4,2,2,2,2,2,2,2,2,2,2,2,2,2,2,2,2,
2,2,2,2,2,2,2,2,2,2,2,2,2,2,2,2,2,2,2,2,2,2,2,2,2,2,2,2,2,2,2,2,2,2,2,2,
2,2,2,2,2,2,2,2,2,2,2,2,2,2,2,2,2,2,2,2,2,2,2,2,2,2,2,2,2,2,2,2,2,2,2,2,
2,2,2,2,2,2,2,4),(-1.95100679492342,-1.94553554215874,-1.94213804667716,
-1.93990677847412,-1.93760342501637,-1.93386827799253,-1.9211061129625,
-1.89205500980332,-1.86516454365593,-1.85721285694531,-1.85281552171066,
-1.8490327262702,-1.84437262323765,-1.83711752238394,-1.79960420208942,
-1.77886519124092,-1.76795054004047,-1.76450259684623,-1.76226086455139,
-1.75997037499978,-1.75629508311787,-1.74420221440886,-1.71467095383175,
-1.68753171550091,-1.6795476308099,-1.67514356190614,-1.67136099812686,
-1.66670883466499,-1.65948140456391,-1.61342297959296,-1.59858137919268,
-1.5897072467776,-1.58650130339884,-1.58430710390816,-1.58194401922727,
-1.57793351072505,-1.5615167452042,-1.52840572645558,-1.5065328814406,-1.50029265420715,
-1.49625140444382,-1.49241959655834,-1.48706498107939,-1.47448297266626,
-1.42888359813295,-1.41329652895715,-1.40945124094734,-1.40712386440035,
-1.40493521178522,-1.40164279743205,-1.39278676886684,-1.3776007473694,
-1.34099707081957,-1.32723999252894,-1.3217014440573,-1.31783681791631,
-1.31384474109794,-1.30784874779921,-1.28885002096639,-1.24763459236768,
-1.23527343263245,-1.2315727575126,-1.22927636683713,-1.22703745359635,
-1.22360767810163,-1.21287322602267,-1.19272101647304,-1.15434161743092,
-1.14714426159606,-1.14249979135334,-1.13871603367635,-1.13430210616619,
-1.1262755604058,-1.09882103744547,-1.06870098323283,-1.05736223775691,
-1.05376093847029,-1.05148614440694,-1.04923168946894,-1.04571900156196,
-1.03416374504659,-1.01122841272118,-0.976885677006135,-0.969525378929181,
-0.964835896402267,-0.961053219295875,-0.95668279022599,-0.948856123583707,
-0.922899839858273,-0.882464950763336,-0.877231291446488,-0.874614949859364,
-0.872693355038265,-0.870058734919367,-0.864737193551888,-0.84317229986637,
-0.832307780531444),.UNSPECIFIED.);
#1510=B_SPLINE_CURVE_WITH_KNOTS('',3,(#25894,#25895,#25896,#25897,#25898,
#25899,#25900,#25901,#25902,#25903,#25904,#25905,#25906,#25907,#25908,#25909,
#25910,#25911,#25912,#25913,#25914,#25915,#25916,#25917,#25918,#25919,#25920,
#25921,#25922,#25923,#25924,#25925,#25926,#25927,#25928,#25929,#25930,#25931,
#25932,#25933,#25934,#25935,#25936,#25937,#25938,#25939,#25940,#25941,#25942,
#25943,#25944,#25945,#25946,#25947,#25948,#25949,#25950,#25951,#25952,#25953,
#25954,#25955,#25956,#25957,#25958,#25959,#25960,#25961,#25962,#25963,#25964,
#25965,#25966,#25967,#25968,#25969,#25970,#25971,#25972,#25973,#25974,#25975,
#25976,#25977,#25978,#25979,#25980,#25981,#25982,#25983,#25984,#25985,#25986,
#25987,#25988,#25989,#25990,#25991,#25992,#25993,#25994,#25995,#25996,#25997,
#25998,#25999,#26000,#26001,#26002,#26003,#26004,#26005,#26006,#26007,#26008,
#26009,#26010,#26011,#26012,#26013,#26014,#26015,#26016,#26017,#26018,#26019,
#26020,#26021,#26022,#26023,#26024,#26025,#26026,#26027,#26028,#26029),
 .UNSPECIFIED.,.F.,.F.,(4,2,2,2,2,2,2,2,2,2,2,2,2,2,2,2,2,2,2,2,2,2,2,2,
2,2,2,2,2,2,2,2,2,2,2,2,2,2,2,2,2,2,2,2,2,2,2,2,2,2,2,2,2,2,2,2,2,2,2,2,
2,2,2,2,2,2,2,4),(-0.832307780531444,-0.803606962550582,-0.792532170867328,
-0.787604593523706,-0.783784651759978,-0.779597549081722,-0.772669392876491,
-0.736864982324837,-0.704657593195993,-0.699432919648634,-0.696815583722776,
-0.694888675712656,-0.692239894271248,-0.686870239755252,-0.664899577261703,
-0.623967025926869,-0.614309574681314,-0.609574598285637,-0.605779361378094,
-0.601420409921478,-0.59368514277229,-0.568473347132404,-0.53078202781163,
-0.523131006997847,-0.520017135668432,-0.517841181344571,-0.515459817405454,
-0.511318375460975,-0.489224089921067,-0.453364914229101,-0.438613909661366,
-0.432952124786665,-0.429433073020253,-0.425561083238544,-0.420101227587134,
-0.405685289338776,-0.38210524528157,-0.348919550486812,-0.343768735724256,
-0.341174915133529,-0.339059128014593,-0.336300366826654,-0.33034234242747,
-0.32196005697253,-0.295896905419883,-0.265630080528906,-0.25816004805516,
-0.25342267499459,-0.249614257711656,-0.245227481539917,-0.237405466381312,
-0.211605047688619,-0.171183813116732,-0.165958067294306,-0.163327191202409,
-0.161148882230516,-0.158303798009289,-0.152045195291431,-0.14310176820436,
-0.113102447558771,-0.0868888313403523,-0.0802339149149218,-0.0760706983808306,
-0.0721754751008024,-0.0669130928135195,-0.0543151460759675,-0.0354023257144985,
-8.33025589524125E-5),.UNSPECIFIED.);
#1511=B_SPLINE_CURVE_WITH_KNOTS('',3,(#26033,#26034,#26035,#26036,#26037,
#26038,#26039,#26040,#26041,#26042,#26043,#26044,#26045,#26046,#26047,#26048,
#26049,#26050,#26051,#26052,#26053,#26054,#26055,#26056,#26057,#26058,#26059,
#26060,#26061,#26062,#26063,#26064,#26065,#26066,#26067,#26068,#26069,#26070,
#26071,#26072,#26073,#26074,#26075,#26076,#26077,#26078,#26079,#26080,#26081,
#26082,#26083,#26084,#26085,#26086,#26087,#26088,#26089,#26090,#26091,#26092),
 .UNSPECIFIED.,.F.,.F.,(4,2,2,2,2,2,2,2,2,2,2,2,2,2,2,2,2,2,2,2,2,2,2,2,
2,2,2,2,2,4),(9.3173987231798E-5,0.0292812570885843,0.0454952117975465,
0.0567410279340209,0.0615976477439388,0.0652310829591134,0.0691415936521615,
0.0754297094370028,0.0985636797155863,0.13271691496439,0.1421093260704,
0.146574060412193,0.150075744261853,0.152251280319118,0.154401966945945,
0.15748619652452,0.164866877593732,0.176361847037279,0.221040972857858,
0.238352711784817,0.244744219454318,0.248677461565565,0.252990814812306,
0.259080628847928,0.274571258417318,0.297181812282976,0.321068730177084,
0.325774599264223,0.327856094682295,0.329629722149541),.UNSPECIFIED.);
#1512=B_SPLINE_CURVE_WITH_KNOTS('',3,(#26093,#26094,#26095,#26096,#26097,
#26098,#26099,#26100,#26101,#26102,#26103,#26104,#26105,#26106,#26107,#26108,
#26109,#26110,#26111,#26112,#26113,#26114,#26115,#26116,#26117,#26118,#26119,
#26120,#26121,#26122,#26123,#26124,#26125,#26126,#26127,#26128,#26129,#26130,
#26131,#26132,#26133,#26134,#26135,#26136,#26137,#26138),.UNSPECIFIED.,
 .F.,.F.,(4,3,3,3,3,3,3,3,3,3,3,3,3,3,3,4),(95.7916386070333,95.90709073475,
96.0227926009489,96.1389321454556,96.2444160663824,96.3525294056605,96.4637895762893,
96.5716115215476,96.6793694345904,96.7871019690566,96.8948477359185,97.0027147634683,
97.1106552609226,97.2187783742407,97.2426107706909,97.3893722612835),
 .UNSPECIFIED.);
#1513=B_SPLINE_CURVE_WITH_KNOTS('',3,(#26146,#26147,#26148,#26149,#26150,
#26151,#26152,#26153,#26154,#26155,#26156,#26157,#26158,#26159,#26160,#26161,
#26162,#26163,#26164,#26165,#26166,#26167,#26168,#26169,#26170,#26171,#26172,
#26173,#26174,#26175,#26176,#26177,#26178,#26179,#26180,#26181,#26182,#26183,
#26184,#26185,#26186,#26187,#26188,#26189,#26190,#26191,#26192,#26193,#26194,
#26195,#26196,#26197,#26198,#26199,#26200,#26201,#26202,#26203,#26204,#26205,
#26206,#26207,#26208,#26209,#26210,#26211,#26212,#26213,#26214,#26215,#26216,
#26217,#26218,#26219,#26220,#26221,#26222,#26223,#26224,#26225,#26226,#26227,
#26228,#26229,#26230,#26231,#26232,#26233,#26234,#26235,#26236,#26237,#26238,
#26239,#26240,#26241,#26242,#26243,#26244,#26245,#26246,#26247,#26248,#26249,
#26250,#26251,#26252,#26253,#26254,#26255,#26256,#26257,#26258,#26259,#26260,
#26261,#26262,#26263,#26264,#26265,#26266,#26267,#26268,#26269,#26270,#26271,
#26272,#26273,#26274,#26275,#26276,#26277,#26278,#26279,#26280,#26281,#26282,
#26283,#26284,#26285,#26286,#26287,#26288,#26289,#26290,#26291,#26292,#26293,
#26294,#26295,#26296,#26297,#26298,#26299,#26300,#26301,#26302,#26303,#26304,
#26305,#26306,#26307,#26308,#26309,#26310,#26311,#26312,#26313,#26314,#26315,
#26316,#26317,#26318,#26319,#26320,#26321,#26322,#26323,#26324,#26325,#26326),
 .UNSPECIFIED.,.F.,.F.,(4,3,3,3,3,3,3,3,3,3,3,3,3,3,3,3,3,3,3,3,3,3,3,3,
3,3,3,3,3,3,3,3,3,3,3,3,3,3,3,3,3,3,3,3,3,3,3,3,3,3,3,3,3,3,3,3,3,3,3,3,
4),(77.7119313453268,77.8591869360628,77.9615391956776,78.0637410289376,
78.165823297785,78.2678407930593,78.3698265486816,78.4718135562898,78.5739050791433,
78.6760500242308,78.7783777791865,78.8573816403713,78.9597691695305,79.0620062241828,
79.1641234778989,79.2661757966064,79.3681961664517,79.4702175311155,79.5723427771074,
79.6745211468974,79.7768814598886,79.8555763446798,79.9579596081616,80.0601927548315,
80.1623066471868,80.2643559400271,80.3663736207563,80.4683926346484,80.5705160644065,
80.6726929115159,80.7750521951542,80.8537710489883,80.9560238596925,81.0581259805397,
81.1601086101123,81.2620265559288,81.363912988911,81.4658010378375,81.567794847017,
81.669842611414,81.7720751652035,81.8519657532968,81.9545178689531,82.056919116762,
82.1591991976819,82.2614134219783,82.3635945480862,82.4657752909354,82.5680566830683,
82.6703896429752,82.7729002617409,82.8501604576053,82.9514894633638,83.0544770780961,
83.1555435477812,83.2565511171417,83.3575340696214,83.4619981475216,83.5630941776532,
83.6692422794376,83.7753903812219),.UNSPECIFIED.);
#1514=B_SPLINE_CURVE_WITH_KNOTS('',3,(#26329,#26330,#26331,#26332,#26333,
#26334,#26335,#26336,#26337,#26338,#26339,#26340,#26341,#26342,#26343,#26344,
#26345,#26346,#26347,#26348,#26349,#26350,#26351,#26352,#26353,#26354,#26355,
#26356,#26357,#26358,#26359,#26360,#26361,#26362,#26363,#26364,#26365,#26366,
#26367,#26368,#26369,#26370,#26371,#26372,#26373,#26374,#26375,#26376,#26377,
#26378,#26379,#26380,#26381,#26382,#26383,#26384,#26385,#26386,#26387,#26388,
#26389,#26390,#26391,#26392,#26393,#26394,#26395,#26396,#26397,#26398,#26399,
#26400,#26401,#26402,#26403,#26404,#26405,#26406,#26407,#26408,#26409,#26410,
#26411,#26412,#26413,#26414,#26415,#26416,#26417,#26418,#26419,#26420,#26421,
#26422,#26423,#26424,#26425,#26426,#26427,#26428,#26429,#26430,#26431,#26432,
#26433,#26434,#26435,#26436,#26437,#26438,#26439,#26440,#26441,#26442,#26443,
#26444,#26445,#26446,#26447,#26448,#26449,#26450,#26451,#26452,#26453,#26454,
#26455,#26456,#26457,#26458,#26459,#26460,#26461,#26462,#26463,#26464,#26465,
#26466,#26467,#26468,#26469,#26470,#26471,#26472,#26473,#26474,#26475,#26476,
#26477,#26478,#26479,#26480,#26481,#26482),.UNSPECIFIED.,.F.,.F.,(4,3,3,
3,3,3,3,3,3,3,3,3,3,3,3,3,3,3,3,3,3,3,3,3,3,3,3,3,3,3,3,3,3,3,3,3,3,3,3,
3,3,3,3,3,3,3,3,3,3,3,3,4),(-85.8447445705308,-85.7400831110115,-85.6354889468789,
-85.5309076570425,-85.4263287010924,-85.3217250850249,-85.2170697942132,
-85.1122558989224,-85.0073555350632,-84.9022530950634,-84.8465498662224,
-84.7450804571866,-84.6437754871337,-84.5426070737962,-84.4415135370295,
-84.3404606582202,-84.2394142729296,-84.1382691275365,-84.0370754030879,
-83.9356960178488,-83.8483551619139,-83.7459059067046,-83.643607801843,
-83.5414308389324,-83.4393196685829,-83.3372413992224,-83.2351631826449,
-83.1329831398502,-83.030751029681,-82.9283393507923,-82.8501604576054,
-82.7476259452047,-82.6452384015215,-82.5429661432666,-82.4407561340788,
-82.338575621552,-82.2363918932184,-82.1341019724148,-82.0317573913236,
-81.9292302304148,-81.8519657532969,-81.7497073069701,-81.647600809257,
-81.5456157032775,-81.4436964451327,-81.3418098618395,-81.2399228237298,
-81.1379318179721,-81.0358878546504,-80.9336606981718,-80.8537710489884,
-80.6873799771529),.UNSPECIFIED.);
#1515=B_SPLINE_CURVE_WITH_KNOTS('',3,(#26859,#26860,#26861,#26862,#26863,
#26864,#26865,#26866,#26867,#26868,#26869,#26870,#26871,#26872,#26873,#26874,
#26875,#26876,#26877,#26878,#26879,#26880,#26881,#26882,#26883,#26884,#26885,
#26886,#26887,#26888,#26889,#26890,#26891,#26892,#26893,#26894,#26895,#26896,
#26897,#26898,#26899,#26900,#26901,#26902,#26903,#26904,#26905,#26906,#26907,
#26908,#26909,#26910,#26911,#26912,#26913,#26914,#26915,#26916,#26917,#26918,
#26919,#26920,#26921,#26922,#26923,#26924,#26925,#26926,#26927,#26928,#26929,
#26930,#26931,#26932,#26933,#26934,#26935,#26936,#26937,#26938,#26939,#26940),
 .UNSPECIFIED.,.F.,.F.,(4,3,3,3,3,3,3,3,3,3,3,3,3,3,3,3,3,3,3,3,3,3,3,3,
3,3,3,4),(0.,0.0160334974104419,0.0395642075561535,0.0633644118263318,0.0837263817738086,
0.0874470583914756,0.110604406527102,0.133695295125757,0.156786183724411,
0.165329376229777,0.169027049684205,0.19120783931272,0.212732869209134,
0.226227078758941,0.24288151240858,0.246186438911864,0.267772589721302,
0.289583909371892,0.305496742371809,0.315196008042082,0.319047580844878,
0.340135104073168,0.359186757307379,0.366235629765007,0.370741076209788,
0.390853652067857,0.410818111358785,0.415993328865216),.UNSPECIFIED.);
#1516=B_SPLINE_CURVE_WITH_KNOTS('',3,(#26942,#26943,#26944,#26945,#26946,
#26947,#26948,#26949,#26950,#26951,#26952,#26953,#26954,#26955,#26956,#26957,
#26958,#26959,#26960,#26961,#26962,#26963,#26964,#26965,#26966,#26967,#26968,
#26969,#26970,#26971,#26972,#26973,#26974,#26975,#26976,#26977,#26978,#26979,
#26980,#26981,#26982,#26983,#26984,#26985,#26986,#26987,#26988,#26989,#26990,
#26991,#26992,#26993,#26994,#26995,#26996,#26997,#26998,#26999,#27000,#27001,
#27002,#27003,#27004,#27005,#27006,#27007,#27008,#27009,#27010,#27011,#27012,
#27013,#27014,#27015,#27016,#27017,#27018,#27019,#27020,#27021,#27022,#27023),
 .UNSPECIFIED.,.F.,.F.,(4,3,3,3,3,3,3,3,3,3,3,3,3,3,3,3,3,3,3,3,3,3,3,3,
3,3,3,4),(-0.415993328865187,-0.402901270545643,-0.382908564831211,-0.371774763313882,
-0.367435224694355,-0.346675516489467,-0.32591580828458,-0.321433315753078,
-0.315781547589586,-0.294240898198231,-0.27242808429252,-0.250757332701903,
-0.244873415404794,-0.24111480505867,-0.218638203108128,-0.211619958938312,
-0.189699687125207,-0.167779415312101,-0.162843814523672,-0.14037333732053,
-0.117486011716815,-0.0943539309902553,-0.0856507589901794,-0.0817563326016671,
-0.0580189261111904,-0.0342375412874052,-0.010964771881335,0.),
 .UNSPECIFIED.);
#1517=B_SPLINE_CURVE_WITH_KNOTS('',3,(#27024,#27025,#27026,#27027),
 .UNSPECIFIED.,.F.,.F.,(4,4),(-0.013270419803488,0.),.UNSPECIFIED.);
#1518=B_SPLINE_CURVE_WITH_KNOTS('',3,(#27029,#27030,#27031,#27032,#27033,
#27034,#27035,#27036,#27037,#27038,#27039,#27040,#27041,#27042,#27043,#27044,
#27045,#27046,#27047,#27048,#27049,#27050,#27051,#27052,#27053,#27054,#27055,
#27056,#27057,#27058,#27059,#27060,#27061,#27062,#27063,#27064,#27065,#27066,
#27067,#27068,#27069,#27070,#27071,#27072,#27073,#27074,#27075,#27076,#27077,
#27078,#27079,#27080,#27081,#27082,#27083,#27084,#27085,#27086,#27087,#27088,
#27089,#27090,#27091,#27092,#27093,#27094,#27095,#27096,#27097,#27098,#27099,
#27100,#27101,#27102,#27103,#27104,#27105,#27106,#27107,#27108,#27109,#27110,
#27111,#27112,#27113,#27114,#27115,#27116),.UNSPECIFIED.,.F.,.F.,(4,3,3,
3,3,3,3,3,3,3,3,3,3,3,3,3,3,3,3,3,3,3,3,3,3,3,3,3,3,4),(-0.410048543780163,
-0.398139186466655,-0.374410169279448,-0.362901775202635,-0.357252904496043,
-0.353226071091677,-0.329831664546775,-0.312242260164576,-0.303769719034645,
-0.299630020912383,-0.276842045832635,-0.254514602197622,-0.232670178061085,
-0.225307920334055,-0.221146019951397,-0.21755552666877,-0.195982423127032,
-0.189116736674495,-0.166997686104259,-0.146198385794381,-0.141443407849317,
-0.12001432471249,-0.0987103641811844,-0.0775869942730841,-0.0725417907976872,
-0.0674800293840683,-0.0468865361744227,-0.0269015552315733,-0.00767557047989959,
0.),.UNSPECIFIED.);
#1519=B_SPLINE_CURVE_WITH_KNOTS('',3,(#27474,#27475,#27476,#27477,#27478,
#27479,#27480,#27481,#27482,#27483,#27484,#27485,#27486,#27487,#27488,#27489,
#27490,#27491,#27492,#27493,#27494,#27495,#27496,#27497,#27498,#27499,#27500,
#27501,#27502,#27503,#27504,#27505,#27506,#27507,#27508,#27509,#27510,#27511,
#27512,#27513,#27514,#27515,#27516,#27517,#27518,#27519,#27520,#27521,#27522,
#27523,#27524,#27525,#27526,#27527,#27528,#27529,#27530,#27531,#27532,#27533,
#27534,#27535,#27536,#27537,#27538,#27539,#27540,#27541,#27542,#27543,#27544,
#27545,#27546,#27547,#27548,#27549,#27550,#27551,#27552,#27553,#27554,#27555,
#27556,#27557,#27558,#27559,#27560,#27561),.UNSPECIFIED.,.F.,.F.,(4,3,3,
3,3,3,3,3,3,3,3,3,3,3,3,3,3,3,3,3,3,3,3,3,3,3,3,3,3,4),(0.,0.0130464519754968,
0.0327301024266493,0.0529569041528836,0.0626751748968586,0.0683819350422815,
0.0728898740513483,0.0938311318830955,0.115156107462477,0.136611032509031,
0.143309507195499,0.146634619759991,0.168716970870795,0.190720450842287,
0.203657142534596,0.22030049657604,0.223957438687906,0.245741331031745,
0.268250311172619,0.290759291313493,0.295289317391233,0.299519479633725,
0.303835795791196,0.327161928089292,0.350378655359791,0.356293009821619,
0.360744190415631,0.384491412450957,0.408026460803736,0.414097116159586),
 .UNSPECIFIED.);
#1520=B_SPLINE_CURVE_WITH_KNOTS('',3,(#27562,#27563,#27564,#27565),
 .UNSPECIFIED.,.F.,.F.,(4,4),(0.,0.0132705018374832),.UNSPECIFIED.);
#1521=VERTEX_POINT('',#5160);
#1522=VERTEX_POINT('',#5161);
#1523=VERTEX_POINT('',#5176);
#1524=VERTEX_POINT('',#5178);
#1525=VERTEX_POINT('',#5195);
#1526=VERTEX_POINT('',#5197);
#1527=VERTEX_POINT('',#5228);
#1528=VERTEX_POINT('',#5243);
#1529=VERTEX_POINT('',#5263);
#1530=VERTEX_POINT('',#5264);
#1531=VERTEX_POINT('',#5266);
#1532=VERTEX_POINT('',#5268);
#1533=VERTEX_POINT('',#5272);
#1534=VERTEX_POINT('',#5274);
#1535=VERTEX_POINT('',#5278);
#1536=VERTEX_POINT('',#5280);
#1537=VERTEX_POINT('',#5284);
#1538=VERTEX_POINT('',#5286);
#1539=VERTEX_POINT('',#5290);
#1540=VERTEX_POINT('',#5292);
#1541=VERTEX_POINT('',#5302);
#1542=VERTEX_POINT('',#5303);
#1543=VERTEX_POINT('',#5340);
#1544=VERTEX_POINT('',#5342);
#1545=VERTEX_POINT('',#5380);
#1546=VERTEX_POINT('',#5382);
#1547=VERTEX_POINT('',#5386);
#1548=VERTEX_POINT('',#5389);
#1549=VERTEX_POINT('',#5393);
#1550=VERTEX_POINT('',#5397);
#1551=VERTEX_POINT('',#5401);
#1552=VERTEX_POINT('',#5404);
#1553=VERTEX_POINT('',#5408);
#1554=VERTEX_POINT('',#5411);
#1555=VERTEX_POINT('',#5444);
#1556=VERTEX_POINT('',#5445);
#1557=VERTEX_POINT('',#5460);
#1558=VERTEX_POINT('',#5462);
#1559=VERTEX_POINT('',#5479);
#1560=VERTEX_POINT('',#5481);
#1561=VERTEX_POINT('',#5512);
#1562=VERTEX_POINT('',#5527);
#1563=VERTEX_POINT('',#5547);
#1564=VERTEX_POINT('',#5548);
#1565=VERTEX_POINT('',#5550);
#1566=VERTEX_POINT('',#5552);
#1567=VERTEX_POINT('',#5556);
#1568=VERTEX_POINT('',#5558);
#1569=VERTEX_POINT('',#5562);
#1570=VERTEX_POINT('',#5564);
#1571=VERTEX_POINT('',#5568);
#1572=VERTEX_POINT('',#5570);
#1573=VERTEX_POINT('',#5574);
#1574=VERTEX_POINT('',#5576);
#1575=VERTEX_POINT('',#5586);
#1576=VERTEX_POINT('',#5587);
#1577=VERTEX_POINT('',#5596);
#1578=VERTEX_POINT('',#5598);
#1579=VERTEX_POINT('',#5605);
#1580=VERTEX_POINT('',#5607);
#1581=VERTEX_POINT('',#5616);
#1582=VERTEX_POINT('',#5618);
#1583=VERTEX_POINT('',#5627);
#1584=VERTEX_POINT('',#5629);
#1585=VERTEX_POINT('',#5638);
#1586=VERTEX_POINT('',#5640);
#1587=VERTEX_POINT('',#5649);
#1588=VERTEX_POINT('',#5651);
#1589=VERTEX_POINT('',#5660);
#1590=VERTEX_POINT('',#5662);
#1591=VERTEX_POINT('',#5671);
#1592=VERTEX_POINT('',#5673);
#1593=VERTEX_POINT('',#5682);
#1594=VERTEX_POINT('',#5684);
#1595=VERTEX_POINT('',#5693);
#1596=VERTEX_POINT('',#5695);
#1597=VERTEX_POINT('',#5704);
#1598=VERTEX_POINT('',#5706);
#1599=VERTEX_POINT('',#5715);
#1600=VERTEX_POINT('',#5717);
#1601=VERTEX_POINT('',#5726);
#1602=VERTEX_POINT('',#5728);
#1603=VERTEX_POINT('',#5737);
#1604=VERTEX_POINT('',#5739);
#1605=VERTEX_POINT('',#5741);
#1606=VERTEX_POINT('',#5748);
#1607=VERTEX_POINT('',#5750);
#1608=VERTEX_POINT('',#5759);
#1609=VERTEX_POINT('',#5761);
#1610=VERTEX_POINT('',#5770);
#1611=VERTEX_POINT('',#5772);
#1612=VERTEX_POINT('',#5781);
#1613=VERTEX_POINT('',#5783);
#1614=VERTEX_POINT('',#5792);
#1615=VERTEX_POINT('',#5794);
#1616=VERTEX_POINT('',#5803);
#1617=VERTEX_POINT('',#5805);
#1618=VERTEX_POINT('',#5814);
#1619=VERTEX_POINT('',#5816);
#1620=VERTEX_POINT('',#5825);
#1621=VERTEX_POINT('',#5827);
#1622=VERTEX_POINT('',#5836);
#1623=VERTEX_POINT('',#5838);
#1624=VERTEX_POINT('',#5847);
#1625=VERTEX_POINT('',#5849);
#1626=VERTEX_POINT('',#5858);
#1627=VERTEX_POINT('',#5860);
#1628=VERTEX_POINT('',#5869);
#1629=VERTEX_POINT('',#5871);
#1630=VERTEX_POINT('',#5882);
#1631=VERTEX_POINT('',#5883);
#1632=VERTEX_POINT('',#5890);
#1633=VERTEX_POINT('',#5892);
#1634=VERTEX_POINT('',#5901);
#1635=VERTEX_POINT('',#5903);
#1636=VERTEX_POINT('',#5912);
#1637=VERTEX_POINT('',#5914);
#1638=VERTEX_POINT('',#5923);
#1639=VERTEX_POINT('',#5925);
#1640=VERTEX_POINT('',#5934);
#1641=VERTEX_POINT('',#5936);
#1642=VERTEX_POINT('',#5945);
#1643=VERTEX_POINT('',#5947);
#1644=VERTEX_POINT('',#5956);
#1645=VERTEX_POINT('',#5958);
#1646=VERTEX_POINT('',#5967);
#1647=VERTEX_POINT('',#5969);
#1648=VERTEX_POINT('',#5978);
#1649=VERTEX_POINT('',#5980);
#1650=VERTEX_POINT('',#5989);
#1651=VERTEX_POINT('',#5991);
#1652=VERTEX_POINT('',#6000);
#1653=VERTEX_POINT('',#6002);
#1654=VERTEX_POINT('',#6011);
#1655=VERTEX_POINT('',#6013);
#1656=VERTEX_POINT('',#6022);
#1657=VERTEX_POINT('',#6024);
#1658=VERTEX_POINT('',#6026);
#1659=VERTEX_POINT('',#6033);
#1660=VERTEX_POINT('',#6035);
#1661=VERTEX_POINT('',#6044);
#1662=VERTEX_POINT('',#6046);
#1663=VERTEX_POINT('',#6055);
#1664=VERTEX_POINT('',#6057);
#1665=VERTEX_POINT('',#6066);
#1666=VERTEX_POINT('',#6068);
#1667=VERTEX_POINT('',#6077);
#1668=VERTEX_POINT('',#6079);
#1669=VERTEX_POINT('',#6088);
#1670=VERTEX_POINT('',#6090);
#1671=VERTEX_POINT('',#6099);
#1672=VERTEX_POINT('',#6101);
#1673=VERTEX_POINT('',#6110);
#1674=VERTEX_POINT('',#6112);
#1675=VERTEX_POINT('',#6121);
#1676=VERTEX_POINT('',#6123);
#1677=VERTEX_POINT('',#6132);
#1678=VERTEX_POINT('',#6134);
#1679=VERTEX_POINT('',#6143);
#1680=VERTEX_POINT('',#6145);
#1681=VERTEX_POINT('',#6154);
#1682=VERTEX_POINT('',#6156);
#1683=VERTEX_POINT('',#6165);
#1684=VERTEX_POINT('',#6167);
#1685=VERTEX_POINT('',#6178);
#1686=VERTEX_POINT('',#6541);
#1687=VERTEX_POINT('',#6556);
#1688=VERTEX_POINT('',#6580);
#1689=VERTEX_POINT('',#6610);
#1690=VERTEX_POINT('',#7134);
#1691=VERTEX_POINT('',#7617);
#1692=VERTEX_POINT('',#7619);
#1693=VERTEX_POINT('',#7626);
#1694=VERTEX_POINT('',#7628);
#1695=VERTEX_POINT('',#7632);
#1696=VERTEX_POINT('',#7637);
#1697=VERTEX_POINT('',#7643);
#1698=VERTEX_POINT('',#7644);
#1699=VERTEX_POINT('',#7646);
#1700=VERTEX_POINT('',#7834);
#1701=VERTEX_POINT('',#7973);
#1702=VERTEX_POINT('',#7974);
#1703=VERTEX_POINT('',#8317);
#1704=VERTEX_POINT('',#8318);
#1705=VERTEX_POINT('',#8651);
#1706=VERTEX_POINT('',#8652);
#1707=VERTEX_POINT('',#8981);
#1708=VERTEX_POINT('',#8982);
#1709=VERTEX_POINT('',#9317);
#1710=VERTEX_POINT('',#9318);
#1711=VERTEX_POINT('',#9657);
#1712=VERTEX_POINT('',#9684);
#1713=VERTEX_POINT('',#9872);
#1714=VERTEX_POINT('',#9874);
#1715=VERTEX_POINT('',#10042);
#1716=VERTEX_POINT('',#10043);
#1717=VERTEX_POINT('',#10162);
#1718=VERTEX_POINT('',#10164);
#1719=VERTEX_POINT('',#10191);
#1720=VERTEX_POINT('',#10520);
#1721=VERTEX_POINT('',#10861);
#1722=VERTEX_POINT('',#11208);
#1723=VERTEX_POINT('',#11438);
#1724=VERTEX_POINT('',#11782);
#1725=VERTEX_POINT('',#12126);
#1726=VERTEX_POINT('',#12206);
#1727=VERTEX_POINT('',#12208);
#1728=VERTEX_POINT('',#12221);
#1729=VERTEX_POINT('',#12553);
#1730=VERTEX_POINT('',#12900);
#1731=VERTEX_POINT('',#13244);
#1732=VERTEX_POINT('',#13597);
#1733=VERTEX_POINT('',#14305);
#1734=VERTEX_POINT('',#14306);
#1735=VERTEX_POINT('',#14395);
#1736=VERTEX_POINT('',#14400);
#1737=VERTEX_POINT('',#14489);
#1738=VERTEX_POINT('',#14503);
#1739=VERTEX_POINT('',#14505);
#1740=VERTEX_POINT('',#14539);
#1741=VERTEX_POINT('',#14628);
#1742=VERTEX_POINT('',#14633);
#1743=VERTEX_POINT('',#14721);
#1744=VERTEX_POINT('',#14725);
#1745=VERTEX_POINT('',#15027);
#1746=VERTEX_POINT('',#15321);
#1747=VERTEX_POINT('',#15521);
#1748=VERTEX_POINT('',#15523);
#1749=VERTEX_POINT('',#15531);
#1750=VERTEX_POINT('',#15533);
#1751=VERTEX_POINT('',#15537);
#1752=VERTEX_POINT('',#15540);
#1753=VERTEX_POINT('',#15544);
#1754=VERTEX_POINT('',#15545);
#1755=VERTEX_POINT('',#15582);
#1756=VERTEX_POINT('',#15584);
#1757=VERTEX_POINT('',#15622);
#1758=VERTEX_POINT('',#15624);
#1759=VERTEX_POINT('',#15628);
#1760=VERTEX_POINT('',#15631);
#1761=VERTEX_POINT('',#15633);
#1762=VERTEX_POINT('',#15637);
#1763=VERTEX_POINT('',#15641);
#1764=VERTEX_POINT('',#15647);
#1765=VERTEX_POINT('',#15651);
#1766=VERTEX_POINT('',#15655);
#1767=VERTEX_POINT('',#15659);
#1768=VERTEX_POINT('',#15662);
#1769=VERTEX_POINT('',#15666);
#1770=VERTEX_POINT('',#15669);
#1771=VERTEX_POINT('',#15673);
#1772=VERTEX_POINT('',#15677);
#1773=VERTEX_POINT('',#15681);
#1774=VERTEX_POINT('',#15685);
#1775=VERTEX_POINT('',#15689);
#1776=VERTEX_POINT('',#15692);
#1777=VERTEX_POINT('',#15696);
#1778=VERTEX_POINT('',#15703);
#1779=VERTEX_POINT('',#15705);
#1780=VERTEX_POINT('',#15709);
#1781=VERTEX_POINT('',#15714);
#1782=VERTEX_POINT('',#15720);
#1783=VERTEX_POINT('',#15721);
#1784=VERTEX_POINT('',#15723);
#1785=VERTEX_POINT('',#15728);
#1786=VERTEX_POINT('',#15853);
#1787=VERTEX_POINT('',#15860);
#1788=VERTEX_POINT('',#15862);
#1789=VERTEX_POINT('',#15865);
#1790=VERTEX_POINT('',#15937);
#1791=VERTEX_POINT('',#15938);
#1792=VERTEX_POINT('',#15976);
#1793=VERTEX_POINT('',#15977);
#1794=VERTEX_POINT('',#16400);
#1795=VERTEX_POINT('',#16401);
#1796=VERTEX_POINT('',#16800);
#1797=VERTEX_POINT('',#16801);
#1798=VERTEX_POINT('',#16803);
#1799=VERTEX_POINT('',#17018);
#1800=VERTEX_POINT('',#17234);
#1801=VERTEX_POINT('',#17235);
#1802=VERTEX_POINT('',#17237);
#1803=VERTEX_POINT('',#17442);
#1804=VERTEX_POINT('',#17646);
#1805=VERTEX_POINT('',#17647);
#1806=VERTEX_POINT('',#18050);
#1807=VERTEX_POINT('',#18051);
#1808=VERTEX_POINT('',#18053);
#1809=VERTEX_POINT('',#18258);
#1810=VERTEX_POINT('',#18468);
#1811=VERTEX_POINT('',#18469);
#1812=VERTEX_POINT('',#18870);
#1813=VERTEX_POINT('',#18871);
#1814=VERTEX_POINT('',#19294);
#1815=VERTEX_POINT('',#19295);
#1816=VERTEX_POINT('',#19297);
#1817=VERTEX_POINT('',#19496);
#1818=VERTEX_POINT('',#19718);
#1819=VERTEX_POINT('',#19719);
#1820=VERTEX_POINT('',#19721);
#1821=VERTEX_POINT('',#19932);
#1822=VERTEX_POINT('',#20144);
#1823=VERTEX_POINT('',#20145);
#1824=VERTEX_POINT('',#20552);
#1825=VERTEX_POINT('',#20553);
#1826=VERTEX_POINT('',#20958);
#1827=VERTEX_POINT('',#20959);
#1828=VERTEX_POINT('',#20961);
#1829=VERTEX_POINT('',#21112);
#1830=VERTEX_POINT('',#21257);
#1831=VERTEX_POINT('',#21258);
#1832=VERTEX_POINT('',#21633);
#1833=VERTEX_POINT('',#21634);
#1834=VERTEX_POINT('',#21636);
#1835=VERTEX_POINT('',#22034);
#1836=VERTEX_POINT('',#22035);
#1837=VERTEX_POINT('',#22416);
#1838=VERTEX_POINT('',#22417);
#1839=VERTEX_POINT('',#22802);
#1840=VERTEX_POINT('',#22803);
#1841=VERTEX_POINT('',#23194);
#1842=VERTEX_POINT('',#23195);
#1843=VERTEX_POINT('',#23576);
#1844=VERTEX_POINT('',#23577);
#1845=VERTEX_POINT('',#23966);
#1846=VERTEX_POINT('',#23967);
#1847=VERTEX_POINT('',#24344);
#1848=VERTEX_POINT('',#24345);
#1849=VERTEX_POINT('',#24730);
#1850=VERTEX_POINT('',#24731);
#1851=VERTEX_POINT('',#25114);
#1852=VERTEX_POINT('',#25115);
#1853=VERTEX_POINT('',#25309);
#1854=VERTEX_POINT('',#25505);
#1855=VERTEX_POINT('',#25506);
#1856=VERTEX_POINT('',#25893);
#1857=VERTEX_POINT('',#26030);
#1858=VERTEX_POINT('',#26032);
#1859=VERTEX_POINT('',#26140);
#1860=VERTEX_POINT('',#26145);
#1861=VERTEX_POINT('',#26327);
#1862=VERTEX_POINT('',#26484);
#1863=VERTEX_POINT('',#26486);
#1864=VERTEX_POINT('',#26489);
#1865=VERTEX_POINT('',#26491);
#1866=VERTEX_POINT('',#26495);
#1867=VERTEX_POINT('',#26501);
#1868=VERTEX_POINT('',#26941);
#1869=VERTEX_POINT('',#27473);
#1870=VERTEX_POINT('',#27568);
#1871=VERTEX_POINT('',#27570);
#1872=VERTEX_POINT('',#27574);
#1873=VERTEX_POINT('',#27579);
#1874=VERTEX_POINT('',#27581);
#1875=VERTEX_POINT('',#27585);
#1876=VERTEX_POINT('',#27590);
#1877=VERTEX_POINT('',#27594);
#1878=VERTEX_POINT('',#27597);
#1879=VERTEX_POINT('',#27599);
#1880=VERTEX_POINT('',#27603);
#1881=VERTEX_POINT('',#27607);
#1882=VERTEX_POINT('',#27612);
#1883=VERTEX_POINT('',#27616);
#1884=VERTEX_POINT('',#27620);
#1885=VERTEX_POINT('',#27624);
#1886=VERTEX_POINT('',#27627);
#1887=VERTEX_POINT('',#27629);
#1888=VERTEX_POINT('',#27633);
#1889=VERTEX_POINT('',#27637);
#1890=VERTEX_POINT('',#27640);
#1891=VERTEX_POINT('',#27644);
#1892=VERTEX_POINT('',#27647);
#1893=VERTEX_POINT('',#27649);
#1894=VERTEX_POINT('',#27661);
#1895=VERTEX_POINT('',#27663);
#1896=VERTEX_POINT('',#27667);
#1897=VERTEX_POINT('',#27670);
#1898=EDGE_CURVE('',#1521,#1522,#1267,.T.);
#1899=EDGE_CURVE('',#1522,#1523,#915,.T.);
#1900=EDGE_CURVE('',#1524,#1523,#1268,.T.);
#1901=EDGE_CURVE('',#1521,#1524,#916,.T.);
#1902=EDGE_CURVE('',#1525,#1521,#218,.T.);
#1903=EDGE_CURVE('',#1526,#1524,#219,.T.);
#1904=EDGE_CURVE('',#1525,#1526,#917,.T.);
#1905=EDGE_CURVE('',#1527,#1525,#1269,.T.);
#1906=EDGE_CURVE('',#1528,#1526,#1270,.T.);
#1907=EDGE_CURVE('',#1527,#1528,#918,.T.);
#1908=EDGE_CURVE('',#1522,#1527,#220,.T.);
#1909=EDGE_CURVE('',#1523,#1528,#221,.T.);
#1910=EDGE_CURVE('',#1529,#1530,#919,.T.);
#1911=EDGE_CURVE('',#1530,#1531,#920,.T.);
#1912=EDGE_CURVE('',#1532,#1531,#921,.T.);
#1913=EDGE_CURVE('',#1529,#1532,#922,.T.);
#1914=EDGE_CURVE('',#1533,#1529,#923,.T.);
#1915=EDGE_CURVE('',#1534,#1532,#924,.T.);
#1916=EDGE_CURVE('',#1533,#1534,#925,.T.);
#1917=EDGE_CURVE('',#1535,#1533,#926,.T.);
#1918=EDGE_CURVE('',#1536,#1534,#927,.T.);
#1919=EDGE_CURVE('',#1535,#1536,#928,.T.);
#1920=EDGE_CURVE('',#1537,#1535,#929,.T.);
#1921=EDGE_CURVE('',#1538,#1536,#930,.T.);
#1922=EDGE_CURVE('',#1537,#1538,#931,.T.);
#1923=EDGE_CURVE('',#1539,#1537,#932,.T.);
#1924=EDGE_CURVE('',#1540,#1538,#933,.T.);
#1925=EDGE_CURVE('',#1539,#1540,#934,.T.);
#1926=EDGE_CURVE('',#1530,#1539,#935,.T.);
#1927=EDGE_CURVE('',#1531,#1540,#936,.T.);
#1928=EDGE_CURVE('',#1541,#1542,#1271,.T.);
#1929=EDGE_CURVE('',#1542,#1541,#1272,.T.);
#1930=EDGE_CURVE('',#1542,#1543,#937,.T.);
#1931=EDGE_CURVE('',#1544,#1543,#1273,.T.);
#1932=EDGE_CURVE('',#1543,#1544,#1274,.T.);
#1933=EDGE_CURVE('',#1545,#1545,#222,.T.);
#1934=EDGE_CURVE('',#1545,#1546,#938,.T.);
#1935=EDGE_CURVE('',#1546,#1546,#223,.T.);
#1936=EDGE_CURVE('',#1547,#1547,#224,.T.);
#1937=EDGE_CURVE('',#1548,#1548,#225,.T.);
#1938=EDGE_CURVE('',#1548,#1547,#939,.T.);
#1939=EDGE_CURVE('',#1549,#1549,#226,.T.);
#1940=EDGE_CURVE('',#1549,#1548,#940,.T.);
#1941=EDGE_CURVE('',#1549,#1550,#941,.T.);
#1942=EDGE_CURVE('',#1550,#1550,#227,.T.);
#1943=EDGE_CURVE('',#1551,#1551,#228,.T.);
#1944=EDGE_CURVE('',#1552,#1552,#229,.T.);
#1945=EDGE_CURVE('',#1552,#1551,#942,.T.);
#1946=EDGE_CURVE('',#1553,#1553,#230,.T.);
#1947=EDGE_CURVE('',#1554,#1554,#231,.T.);
#1948=EDGE_CURVE('',#1554,#1553,#943,.T.);
#1949=EDGE_CURVE('',#1555,#1556,#1275,.T.);
#1950=EDGE_CURVE('',#1556,#1557,#944,.T.);
#1951=EDGE_CURVE('',#1558,#1557,#1276,.T.);
#1952=EDGE_CURVE('',#1555,#1558,#945,.T.);
#1953=EDGE_CURVE('',#1559,#1555,#232,.T.);
#1954=EDGE_CURVE('',#1560,#1558,#233,.T.);
#1955=EDGE_CURVE('',#1559,#1560,#946,.T.);
#1956=EDGE_CURVE('',#1561,#1559,#1277,.T.);
#1957=EDGE_CURVE('',#1562,#1560,#1278,.T.);
#1958=EDGE_CURVE('',#1561,#1562,#947,.T.);
#1959=EDGE_CURVE('',#1556,#1561,#234,.T.);
#1960=EDGE_CURVE('',#1557,#1562,#235,.T.);
#1961=EDGE_CURVE('',#1563,#1564,#948,.T.);
#1962=EDGE_CURVE('',#1564,#1565,#949,.T.);
#1963=EDGE_CURVE('',#1566,#1565,#950,.T.);
#1964=EDGE_CURVE('',#1563,#1566,#951,.T.);
#1965=EDGE_CURVE('',#1567,#1563,#952,.T.);
#1966=EDGE_CURVE('',#1568,#1566,#953,.T.);
#1967=EDGE_CURVE('',#1567,#1568,#954,.T.);
#1968=EDGE_CURVE('',#1569,#1567,#955,.T.);
#1969=EDGE_CURVE('',#1570,#1568,#956,.T.);
#1970=EDGE_CURVE('',#1569,#1570,#957,.T.);
#1971=EDGE_CURVE('',#1571,#1569,#958,.T.);
#1972=EDGE_CURVE('',#1572,#1570,#959,.T.);
#1973=EDGE_CURVE('',#1571,#1572,#960,.T.);
#1974=EDGE_CURVE('',#1573,#1571,#961,.T.);
#1975=EDGE_CURVE('',#1574,#1572,#962,.T.);
#1976=EDGE_CURVE('',#1573,#1574,#963,.T.);
#1977=EDGE_CURVE('',#1564,#1573,#964,.T.);
#1978=EDGE_CURVE('',#1565,#1574,#965,.T.);
#1979=EDGE_CURVE('',#1575,#1576,#1279,.T.);
#1980=EDGE_CURVE('',#1575,#1577,#966,.T.);
#1981=EDGE_CURVE('',#1578,#1577,#1280,.T.);
#1982=EDGE_CURVE('',#1579,#1578,#967,.T.);
#1983=EDGE_CURVE('',#1580,#1579,#1281,.T.);
#1984=EDGE_CURVE('',#1581,#1580,#968,.T.);
#1985=EDGE_CURVE('',#1582,#1581,#1282,.T.);
#1986=EDGE_CURVE('',#1583,#1582,#969,.T.);
#1987=EDGE_CURVE('',#1584,#1583,#1283,.T.);
#1988=EDGE_CURVE('',#1585,#1584,#970,.T.);
#1989=EDGE_CURVE('',#1586,#1585,#1284,.T.);
#1990=EDGE_CURVE('',#1587,#1586,#971,.T.);
#1991=EDGE_CURVE('',#1588,#1587,#1285,.T.);
#1992=EDGE_CURVE('',#1589,#1588,#972,.T.);
#1993=EDGE_CURVE('',#1590,#1589,#1286,.T.);
#1994=EDGE_CURVE('',#1591,#1590,#973,.T.);
#1995=EDGE_CURVE('',#1592,#1591,#1287,.T.);
#1996=EDGE_CURVE('',#1593,#1592,#974,.T.);
#1997=EDGE_CURVE('',#1594,#1593,#1288,.T.);
#1998=EDGE_CURVE('',#1595,#1594,#975,.T.);
#1999=EDGE_CURVE('',#1596,#1595,#1289,.T.);
#2000=EDGE_CURVE('',#1597,#1596,#976,.T.);
#2001=EDGE_CURVE('',#1598,#1597,#1290,.T.);
#2002=EDGE_CURVE('',#1599,#1598,#977,.T.);
#2003=EDGE_CURVE('',#1600,#1599,#1291,.T.);
#2004=EDGE_CURVE('',#1601,#1600,#978,.T.);
#2005=EDGE_CURVE('',#1602,#1601,#1292,.T.);
#2006=EDGE_CURVE('',#1603,#1602,#979,.T.);
#2007=EDGE_CURVE('',#1604,#1603,#980,.T.);
#2008=EDGE_CURVE('',#1605,#1604,#1293,.T.);
#2009=EDGE_CURVE('',#1606,#1605,#981,.T.);
#2010=EDGE_CURVE('',#1607,#1606,#1294,.T.);
#2011=EDGE_CURVE('',#1608,#1607,#982,.T.);
#2012=EDGE_CURVE('',#1609,#1608,#1295,.T.);
#2013=EDGE_CURVE('',#1610,#1609,#983,.T.);
#2014=EDGE_CURVE('',#1611,#1610,#1296,.T.);
#2015=EDGE_CURVE('',#1612,#1611,#984,.T.);
#2016=EDGE_CURVE('',#1613,#1612,#1297,.T.);
#2017=EDGE_CURVE('',#1614,#1613,#985,.T.);
#2018=EDGE_CURVE('',#1615,#1614,#1298,.T.);
#2019=EDGE_CURVE('',#1616,#1615,#986,.T.);
#2020=EDGE_CURVE('',#1617,#1616,#1299,.T.);
#2021=EDGE_CURVE('',#1618,#1617,#987,.T.);
#2022=EDGE_CURVE('',#1619,#1618,#1300,.T.);
#2023=EDGE_CURVE('',#1620,#1619,#988,.T.);
#2024=EDGE_CURVE('',#1621,#1620,#1301,.T.);
#2025=EDGE_CURVE('',#1622,#1621,#989,.T.);
#2026=EDGE_CURVE('',#1623,#1622,#1302,.T.);
#2027=EDGE_CURVE('',#1624,#1623,#990,.T.);
#2028=EDGE_CURVE('',#1625,#1624,#1303,.T.);
#2029=EDGE_CURVE('',#1626,#1625,#991,.T.);
#2030=EDGE_CURVE('',#1627,#1626,#1304,.T.);
#2031=EDGE_CURVE('',#1628,#1627,#992,.T.);
#2032=EDGE_CURVE('',#1629,#1628,#1305,.T.);
#2033=EDGE_CURVE('',#1576,#1629,#993,.T.);
#2034=EDGE_CURVE('',#1630,#1631,#1306,.T.);
#2035=EDGE_CURVE('',#1632,#1630,#994,.T.);
#2036=EDGE_CURVE('',#1633,#1632,#1307,.T.);
#2037=EDGE_CURVE('',#1634,#1633,#995,.T.);
#2038=EDGE_CURVE('',#1635,#1634,#1308,.T.);
#2039=EDGE_CURVE('',#1636,#1635,#996,.T.);
#2040=EDGE_CURVE('',#1637,#1636,#1309,.T.);
#2041=EDGE_CURVE('',#1638,#1637,#997,.T.);
#2042=EDGE_CURVE('',#1639,#1638,#1310,.T.);
#2043=EDGE_CURVE('',#1640,#1639,#998,.T.);
#2044=EDGE_CURVE('',#1641,#1640,#1311,.T.);
#2045=EDGE_CURVE('',#1642,#1641,#999,.T.);
#2046=EDGE_CURVE('',#1643,#1642,#1312,.T.);
#2047=EDGE_CURVE('',#1644,#1643,#1000,.T.);
#2048=EDGE_CURVE('',#1645,#1644,#1313,.T.);
#2049=EDGE_CURVE('',#1646,#1645,#1001,.T.);
#2050=EDGE_CURVE('',#1647,#1646,#1314,.T.);
#2051=EDGE_CURVE('',#1648,#1647,#1002,.T.);
#2052=EDGE_CURVE('',#1649,#1648,#1315,.T.);
#2053=EDGE_CURVE('',#1650,#1649,#1003,.T.);
#2054=EDGE_CURVE('',#1651,#1650,#1316,.T.);
#2055=EDGE_CURVE('',#1652,#1651,#1004,.T.);
#2056=EDGE_CURVE('',#1653,#1652,#1317,.T.);
#2057=EDGE_CURVE('',#1654,#1653,#1005,.T.);
#2058=EDGE_CURVE('',#1655,#1654,#1318,.T.);
#2059=EDGE_CURVE('',#1656,#1655,#1006,.T.);
#2060=EDGE_CURVE('',#1657,#1656,#1007,.T.);
#2061=EDGE_CURVE('',#1658,#1657,#1319,.T.);
#2062=EDGE_CURVE('',#1659,#1658,#1008,.T.);
#2063=EDGE_CURVE('',#1660,#1659,#1320,.T.);
#2064=EDGE_CURVE('',#1661,#1660,#1009,.T.);
#2065=EDGE_CURVE('',#1662,#1661,#1321,.T.);
#2066=EDGE_CURVE('',#1663,#1662,#1010,.T.);
#2067=EDGE_CURVE('',#1664,#1663,#1322,.T.);
#2068=EDGE_CURVE('',#1665,#1664,#1011,.T.);
#2069=EDGE_CURVE('',#1666,#1665,#1323,.T.);
#2070=EDGE_CURVE('',#1667,#1666,#1012,.T.);
#2071=EDGE_CURVE('',#1668,#1667,#1324,.T.);
#2072=EDGE_CURVE('',#1669,#1668,#1013,.T.);
#2073=EDGE_CURVE('',#1670,#1669,#1325,.T.);
#2074=EDGE_CURVE('',#1671,#1670,#1014,.T.);
#2075=EDGE_CURVE('',#1672,#1671,#1326,.T.);
#2076=EDGE_CURVE('',#1673,#1672,#1015,.T.);
#2077=EDGE_CURVE('',#1674,#1673,#1327,.T.);
#2078=EDGE_CURVE('',#1675,#1674,#1016,.T.);
#2079=EDGE_CURVE('',#1676,#1675,#1328,.T.);
#2080=EDGE_CURVE('',#1677,#1676,#1017,.T.);
#2081=EDGE_CURVE('',#1678,#1677,#1329,.T.);
#2082=EDGE_CURVE('',#1679,#1678,#1018,.T.);
#2083=EDGE_CURVE('',#1680,#1679,#1330,.T.);
#2084=EDGE_CURVE('',#1681,#1680,#1019,.T.);
#2085=EDGE_CURVE('',#1682,#1681,#1331,.T.);
#2086=EDGE_CURVE('',#1683,#1682,#1020,.T.);
#2087=EDGE_CURVE('',#1684,#1683,#1332,.T.);
#2088=EDGE_CURVE('',#1684,#1631,#1021,.T.);
#2089=EDGE_CURVE('',#1602,#1685,#1333,.T.);
#2090=EDGE_CURVE('',#1603,#1685,#236,.T.);
#2091=EDGE_CURVE('',#1654,#1605,#1334,.T.);
#2092=EDGE_CURVE('',#1653,#1606,#1335,.T.);
#2093=EDGE_CURVE('',#1598,#1661,#1336,.T.);
#2094=EDGE_CURVE('',#1599,#1660,#1337,.T.);
#2095=EDGE_CURVE('',#1650,#1609,#1338,.T.);
#2096=EDGE_CURVE('',#1649,#1610,#1339,.T.);
#2097=EDGE_CURVE('',#1594,#1665,#1340,.T.);
#2098=EDGE_CURVE('',#1595,#1664,#1341,.T.);
#2099=EDGE_CURVE('',#1646,#1613,#1342,.T.);
#2100=EDGE_CURVE('',#1645,#1614,#1343,.T.);
#2101=EDGE_CURVE('',#1590,#1669,#1344,.T.);
#2102=EDGE_CURVE('',#1591,#1668,#1345,.T.);
#2103=EDGE_CURVE('',#1642,#1617,#1346,.T.);
#2104=EDGE_CURVE('',#1641,#1618,#1347,.T.);
#2105=EDGE_CURVE('',#1586,#1673,#1348,.T.);
#2106=EDGE_CURVE('',#1587,#1672,#1349,.T.);
#2107=EDGE_CURVE('',#1638,#1621,#1350,.T.);
#2108=EDGE_CURVE('',#1637,#1622,#1351,.T.);
#2109=EDGE_CURVE('',#1582,#1677,#1352,.T.);
#2110=EDGE_CURVE('',#1583,#1676,#1353,.T.);
#2111=EDGE_CURVE('',#1634,#1625,#1354,.T.);
#2112=EDGE_CURVE('',#1633,#1626,#1355,.T.);
#2113=EDGE_CURVE('',#1578,#1681,#1356,.T.);
#2114=EDGE_CURVE('',#1579,#1680,#1357,.T.);
#2115=EDGE_CURVE('',#1686,#1629,#1358,.T.);
#2116=EDGE_CURVE('',#1687,#1686,#237,.T.);
#2117=EDGE_CURVE('',#1687,#1576,#1359,.T.);
#2118=EDGE_CURVE('',#1688,#1683,#1360,.T.);
#2119=EDGE_CURVE('',#1684,#1688,#67,.T.);
#2120=EDGE_CURVE('',#1689,#1604,#1361,.T.);
#2121=EDGE_CURVE('',#1655,#1689,#1362,.T.);
#2122=EDGE_CURVE('',#1651,#1608,#1363,.T.);
#2123=EDGE_CURVE('',#1647,#1612,#1364,.T.);
#2124=EDGE_CURVE('',#1643,#1616,#1365,.T.);
#2125=EDGE_CURVE('',#1639,#1620,#1366,.T.);
#2126=EDGE_CURVE('',#1635,#1624,#1367,.T.);
#2127=EDGE_CURVE('',#1630,#1628,#1368,.T.);
#2128=EDGE_CURVE('',#1686,#1631,#68,.T.);
#2129=EDGE_CURVE('',#1600,#1659,#1369,.T.);
#2130=EDGE_CURVE('',#1596,#1663,#1370,.T.);
#2131=EDGE_CURVE('',#1592,#1667,#1371,.T.);
#2132=EDGE_CURVE('',#1588,#1671,#1372,.T.);
#2133=EDGE_CURVE('',#1584,#1675,#1373,.T.);
#2134=EDGE_CURVE('',#1580,#1679,#1374,.T.);
#2135=EDGE_CURVE('',#1685,#1657,#1375,.T.);
#2136=EDGE_CURVE('',#1656,#1689,#238,.F.);
#2137=EDGE_CURVE('',#1682,#1690,#1376,.T.);
#2138=EDGE_CURVE('',#1688,#1690,#239,.T.);
#2139=EDGE_CURVE('',#1658,#1601,#1377,.T.);
#2140=EDGE_CURVE('',#1607,#1652,#1378,.T.);
#2141=EDGE_CURVE('',#1662,#1597,#1379,.T.);
#2142=EDGE_CURVE('',#1611,#1648,#1380,.T.);
#2143=EDGE_CURVE('',#1666,#1593,#1381,.T.);
#2144=EDGE_CURVE('',#1615,#1644,#1382,.T.);
#2145=EDGE_CURVE('',#1670,#1589,#1383,.T.);
#2146=EDGE_CURVE('',#1619,#1640,#1384,.T.);
#2147=EDGE_CURVE('',#1674,#1585,#1385,.T.);
#2148=EDGE_CURVE('',#1623,#1636,#1386,.T.);
#2149=EDGE_CURVE('',#1678,#1581,#1387,.T.);
#2150=EDGE_CURVE('',#1627,#1632,#1388,.T.);
#2151=EDGE_CURVE('',#1690,#1577,#69,.T.);
#2152=EDGE_CURVE('',#1575,#1687,#1389,.T.);
#2153=EDGE_CURVE('',#1691,#1691,#240,.T.);
#2154=EDGE_CURVE('',#1691,#1692,#1022,.T.);
#2155=EDGE_CURVE('',#1692,#1692,#241,.T.);
#2156=EDGE_CURVE('',#1693,#1693,#242,.T.);
#2157=EDGE_CURVE('',#1693,#1694,#243,.T.);
#2158=EDGE_CURVE('',#1694,#1694,#244,.T.);
#2159=EDGE_CURVE('',#1694,#1695,#1023,.T.);
#2160=EDGE_CURVE('',#1695,#1695,#245,.T.);
#2161=EDGE_CURVE('',#1695,#1696,#246,.T.);
#2162=EDGE_CURVE('',#1696,#1696,#247,.T.);
#2163=EDGE_CURVE('',#1697,#1698,#1024,.T.);
#2164=EDGE_CURVE('',#1699,#1697,#1390,.T.);
#2165=EDGE_CURVE('',#1700,#1699,#248,.T.);
#2166=EDGE_CURVE('',#1700,#1698,#1391,.T.);
#2167=EDGE_CURVE('',#1701,#1702,#1025,.T.);
#2168=EDGE_CURVE('',#1697,#1701,#1392,.F.);
#2169=EDGE_CURVE('',#1698,#1702,#1393,.T.);
#2170=EDGE_CURVE('',#1703,#1704,#1026,.T.);
#2171=EDGE_CURVE('',#1701,#1703,#1394,.F.);
#2172=EDGE_CURVE('',#1702,#1704,#1395,.T.);
#2173=EDGE_CURVE('',#1705,#1706,#1027,.T.);
#2174=EDGE_CURVE('',#1703,#1705,#1396,.F.);
#2175=EDGE_CURVE('',#1704,#1706,#1397,.T.);
#2176=EDGE_CURVE('',#1707,#1708,#1028,.T.);
#2177=EDGE_CURVE('',#1705,#1707,#1398,.F.);
#2178=EDGE_CURVE('',#1706,#1708,#1399,.T.);
#2179=EDGE_CURVE('',#1709,#1710,#1029,.T.);
#2180=EDGE_CURVE('',#1707,#1709,#1400,.F.);
#2181=EDGE_CURVE('',#1708,#1710,#1401,.T.);
#2182=EDGE_CURVE('',#1710,#1711,#1402,.T.);
#2183=EDGE_CURVE('',#1711,#1712,#1403,.T.);
#2184=EDGE_CURVE('',#1713,#1712,#249,.T.);
#2185=EDGE_CURVE('',#1714,#1713,#1404,.T.);
#2186=EDGE_CURVE('',#1709,#1714,#1405,.F.);
#2187=EDGE_CURVE('',#1715,#1716,#1406,.T.);
#2188=EDGE_CURVE('',#1716,#1717,#250,.F.);
#2189=EDGE_CURVE('',#1717,#1718,#1407,.T.);
#2190=EDGE_CURVE('',#1718,#1719,#1408,.T.);
#2191=EDGE_CURVE('',#1719,#1720,#1409,.T.);
#2192=EDGE_CURVE('',#1720,#1721,#1410,.T.);
#2193=EDGE_CURVE('',#1721,#1722,#1411,.T.);
#2194=EDGE_CURVE('',#1722,#1723,#1412,.T.);
#2195=EDGE_CURVE('',#1723,#1724,#1413,.T.);
#2196=EDGE_CURVE('',#1724,#1725,#1414,.T.);
#2197=EDGE_CURVE('',#1726,#1725,#251,.F.);
#2198=EDGE_CURVE('',#1726,#1727,#1415,.T.);
#2199=EDGE_CURVE('',#1727,#1728,#1416,.T.);
#2200=EDGE_CURVE('',#1728,#1729,#1417,.T.);
#2201=EDGE_CURVE('',#1729,#1730,#1418,.T.);
#2202=EDGE_CURVE('',#1730,#1731,#1419,.T.);
#2203=EDGE_CURVE('',#1731,#1732,#1420,.T.);
#2204=EDGE_CURVE('',#1732,#1715,#1421,.T.);
#2205=EDGE_CURVE('',#1733,#1734,#1422,.T.);
#2206=EDGE_CURVE('',#1733,#1735,#1423,.T.);
#2207=EDGE_CURVE('',#1735,#1736,#1424,.T.);
#2208=EDGE_CURVE('',#1736,#1737,#1425,.T.);
#2209=EDGE_CURVE('',#1734,#1737,#1426,.T.);
#2210=EDGE_CURVE('',#1736,#1738,#252,.T.);
#2211=EDGE_CURVE('',#1738,#1739,#1427,.T.);
#2212=EDGE_CURVE('',#1737,#1739,#253,.T.);
#2213=EDGE_CURVE('',#1739,#1740,#1428,.T.);
#2214=EDGE_CURVE('',#1738,#1741,#1429,.T.);
#2215=EDGE_CURVE('',#1741,#1742,#1430,.T.);
#2216=EDGE_CURVE('',#1742,#1740,#1431,.T.);
#2217=EDGE_CURVE('',#1735,#1743,#254,.T.);
#2218=EDGE_CURVE('',#1743,#1742,#255,.T.);
#2219=EDGE_CURVE('',#1744,#1744,#256,.T.);
#2220=EDGE_CURVE('',#1744,#1743,#1030,.T.);
#2221=EDGE_CURVE('',#1740,#1733,#257,.T.);
#2222=EDGE_CURVE('',#1725,#1713,#1432,.T.);
#2223=EDGE_CURVE('',#1745,#1717,#1433,.T.);
#2224=EDGE_CURVE('',#1745,#1699,#1434,.T.);
#2225=EDGE_CURVE('',#1746,#1726,#1435,.T.);
#2226=EDGE_CURVE('',#1712,#1746,#1436,.T.);
#2227=EDGE_CURVE('',#1716,#1700,#1437,.T.);
#2228=EDGE_CURVE('',#1747,#1747,#258,.T.);
#2229=EDGE_CURVE('',#1747,#1748,#1031,.T.);
#2230=EDGE_CURVE('',#1748,#1748,#259,.T.);
#2231=EDGE_CURVE('',#1749,#1749,#260,.T.);
#2232=EDGE_CURVE('',#1749,#1750,#1032,.T.);
#2233=EDGE_CURVE('',#1750,#1750,#261,.T.);
#2234=EDGE_CURVE('',#1751,#1751,#262,.T.);
#2235=EDGE_CURVE('',#1749,#1752,#1033,.T.);
#2236=EDGE_CURVE('',#1752,#1752,#263,.T.);
#2237=EDGE_CURVE('',#1753,#1754,#1438,.T.);
#2238=EDGE_CURVE('',#1754,#1753,#1439,.T.);
#2239=EDGE_CURVE('',#1754,#1755,#1034,.T.);
#2240=EDGE_CURVE('',#1756,#1755,#1440,.T.);
#2241=EDGE_CURVE('',#1755,#1756,#1441,.T.);
#2242=EDGE_CURVE('',#1757,#1757,#264,.T.);
#2243=EDGE_CURVE('',#1757,#1758,#1035,.T.);
#2244=EDGE_CURVE('',#1758,#1758,#265,.T.);
#2245=EDGE_CURVE('',#1759,#1759,#266,.T.);
#2246=EDGE_CURVE('',#1760,#1760,#267,.T.);
#2247=EDGE_CURVE('',#1760,#1761,#1036,.T.);
#2248=EDGE_CURVE('',#1761,#1761,#268,.T.);
#2249=EDGE_CURVE('',#1762,#1762,#269,.T.);
#2250=EDGE_CURVE('',#1762,#1760,#1037,.T.);
#2251=EDGE_CURVE('',#1762,#1763,#1038,.T.);
#2252=EDGE_CURVE('',#1763,#1763,#270,.T.);
#2253=EDGE_CURVE('',#1752,#1763,#1039,.T.);
#2254=EDGE_CURVE('',#1764,#1764,#271,.T.);
#2255=EDGE_CURVE('',#1764,#1751,#1040,.T.);
#2256=EDGE_CURVE('',#1765,#1765,#272,.T.);
#2257=EDGE_CURVE('',#1765,#1764,#1041,.T.);
#2258=EDGE_CURVE('',#1766,#1766,#273,.T.);
#2259=EDGE_CURVE('',#1766,#1765,#1042,.T.);
#2260=EDGE_CURVE('',#1767,#1767,#274,.T.);
#2261=EDGE_CURVE('',#1768,#1768,#275,.T.);
#2262=EDGE_CURVE('',#1768,#1767,#1043,.T.);
#2263=EDGE_CURVE('',#1769,#1769,#276,.T.);
#2264=EDGE_CURVE('',#1770,#1770,#277,.T.);
#2265=EDGE_CURVE('',#1770,#1769,#1044,.T.);
#2266=EDGE_CURVE('',#1771,#1771,#278,.T.);
#2267=EDGE_CURVE('',#1771,#1770,#1045,.T.);
#2268=EDGE_CURVE('',#1772,#1772,#279,.T.);
#2269=EDGE_CURVE('',#1772,#1771,#1046,.T.);
#2270=EDGE_CURVE('',#1773,#1773,#280,.T.);
#2271=EDGE_CURVE('',#1773,#1772,#1047,.T.);
#2272=EDGE_CURVE('',#1774,#1774,#281,.T.);
#2273=EDGE_CURVE('',#1774,#1773,#1048,.T.);
#2274=EDGE_CURVE('',#1775,#1775,#282,.T.);
#2275=EDGE_CURVE('',#1776,#1776,#283,.T.);
#2276=EDGE_CURVE('',#1776,#1775,#1049,.T.);
#2277=EDGE_CURVE('',#1777,#1777,#284,.T.);
#2278=EDGE_CURVE('',#1759,#1777,#1050,.T.);
#2279=EDGE_CURVE('',#1778,#1778,#285,.T.);
#2280=EDGE_CURVE('',#1778,#1779,#286,.T.);
#2281=EDGE_CURVE('',#1779,#1779,#287,.T.);
#2282=EDGE_CURVE('',#1779,#1780,#1051,.T.);
#2283=EDGE_CURVE('',#1780,#1780,#288,.T.);
#2284=EDGE_CURVE('',#1780,#1781,#289,.T.);
#2285=EDGE_CURVE('',#1781,#1781,#290,.T.);
#2286=EDGE_CURVE('',#1782,#1783,#1052,.T.);
#2287=EDGE_CURVE('',#1782,#1784,#1442,.T.);
#2288=EDGE_CURVE('',#1784,#1785,#1443,.T.);
#2289=EDGE_CURVE('',#1785,#1786,#1444,.T.);
#2290=EDGE_CURVE('',#1786,#1787,#291,.T.);
#2291=EDGE_CURVE('',#1787,#1788,#1053,.T.);
#2292=EDGE_CURVE('',#1788,#1788,#292,.F.);
#2293=EDGE_CURVE('',#1787,#1789,#293,.T.);
#2294=EDGE_CURVE('',#1789,#1783,#1445,.T.);
#2295=EDGE_CURVE('',#1790,#1791,#1446,.T.);
#2296=EDGE_CURVE('',#1791,#1790,#1447,.T.);
#2297=EDGE_CURVE('',#1792,#1793,#1054,.T.);
#2298=EDGE_CURVE('',#1792,#1782,#1448,.T.);
#2299=EDGE_CURVE('',#1783,#1793,#1449,.T.);
#2300=EDGE_CURVE('',#1794,#1795,#1055,.T.);
#2301=EDGE_CURVE('',#1794,#1792,#1450,.T.);
#2302=EDGE_CURVE('',#1793,#1795,#1451,.T.);
#2303=EDGE_CURVE('',#1796,#1797,#1056,.T.);
#2304=EDGE_CURVE('',#1796,#1798,#1452,.T.);
#2305=EDGE_CURVE('',#1798,#1794,#1453,.T.);
#2306=EDGE_CURVE('',#1795,#1799,#1454,.T.);
#2307=EDGE_CURVE('',#1799,#1797,#1455,.T.);
#2308=EDGE_CURVE('',#1800,#1801,#1057,.T.);
#2309=EDGE_CURVE('',#1800,#1802,#1456,.T.);
#2310=EDGE_CURVE('',#1802,#1796,#1457,.T.);
#2311=EDGE_CURVE('',#1797,#1803,#1458,.T.);
#2312=EDGE_CURVE('',#1803,#1801,#1459,.T.);
#2313=EDGE_CURVE('',#1804,#1805,#1058,.T.);
#2314=EDGE_CURVE('',#1804,#1800,#1460,.T.);
#2315=EDGE_CURVE('',#1801,#1805,#1461,.T.);
#2316=EDGE_CURVE('',#1806,#1807,#1059,.T.);
#2317=EDGE_CURVE('',#1806,#1808,#1462,.T.);
#2318=EDGE_CURVE('',#1808,#1804,#1463,.T.);
#2319=EDGE_CURVE('',#1805,#1809,#1464,.T.);
#2320=EDGE_CURVE('',#1809,#1807,#1465,.T.);
#2321=EDGE_CURVE('',#1810,#1811,#1060,.T.);
#2322=EDGE_CURVE('',#1810,#1806,#1466,.T.);
#2323=EDGE_CURVE('',#1807,#1811,#1467,.T.);
#2324=EDGE_CURVE('',#1812,#1813,#1061,.T.);
#2325=EDGE_CURVE('',#1812,#1810,#1468,.T.);
#2326=EDGE_CURVE('',#1811,#1813,#1469,.T.);
#2327=EDGE_CURVE('',#1814,#1815,#1062,.T.);
#2328=EDGE_CURVE('',#1814,#1816,#1470,.T.);
#2329=EDGE_CURVE('',#1816,#1812,#1471,.T.);
#2330=EDGE_CURVE('',#1813,#1817,#1472,.T.);
#2331=EDGE_CURVE('',#1817,#1815,#1473,.T.);
#2332=EDGE_CURVE('',#1818,#1819,#1063,.T.);
#2333=EDGE_CURVE('',#1818,#1820,#1474,.T.);
#2334=EDGE_CURVE('',#1820,#1814,#1475,.T.);
#2335=EDGE_CURVE('',#1815,#1821,#1476,.T.);
#2336=EDGE_CURVE('',#1821,#1819,#1477,.T.);
#2337=EDGE_CURVE('',#1822,#1823,#1064,.T.);
#2338=EDGE_CURVE('',#1822,#1818,#1478,.T.);
#2339=EDGE_CURVE('',#1819,#1823,#1479,.T.);
#2340=EDGE_CURVE('',#1824,#1825,#1065,.T.);
#2341=EDGE_CURVE('',#1824,#1822,#1480,.T.);
#2342=EDGE_CURVE('',#1823,#1825,#1481,.T.);
#2343=EDGE_CURVE('',#1826,#1827,#1066,.T.);
#2344=EDGE_CURVE('',#1828,#1826,#1482,.F.);
#2345=EDGE_CURVE('',#1829,#1828,#294,.T.);
#2346=EDGE_CURVE('',#1829,#1827,#1483,.T.);
#2347=EDGE_CURVE('',#1830,#1831,#1067,.T.);
#2348=EDGE_CURVE('',#1826,#1830,#1484,.F.);
#2349=EDGE_CURVE('',#1827,#1831,#1485,.T.);
#2350=EDGE_CURVE('',#1832,#1833,#1068,.T.);
#2351=EDGE_CURVE('',#1834,#1832,#1486,.F.);
#2352=EDGE_CURVE('',#1830,#1834,#1487,.F.);
#2353=EDGE_CURVE('',#1831,#1833,#1488,.T.);
#2354=EDGE_CURVE('',#1835,#1836,#1069,.T.);
#2355=EDGE_CURVE('',#1832,#1835,#1489,.F.);
#2356=EDGE_CURVE('',#1833,#1836,#1490,.T.);
#2357=EDGE_CURVE('',#1837,#1838,#1070,.T.);
#2358=EDGE_CURVE('',#1835,#1837,#1491,.F.);
#2359=EDGE_CURVE('',#1836,#1838,#1492,.T.);
#2360=EDGE_CURVE('',#1839,#1840,#1071,.T.);
#2361=EDGE_CURVE('',#1837,#1839,#1493,.F.);
#2362=EDGE_CURVE('',#1838,#1840,#1494,.T.);
#2363=EDGE_CURVE('',#1841,#1842,#1072,.T.);
#2364=EDGE_CURVE('',#1839,#1841,#1495,.F.);
#2365=EDGE_CURVE('',#1840,#1842,#1496,.T.);
#2366=EDGE_CURVE('',#1843,#1844,#1073,.T.);
#2367=EDGE_CURVE('',#1841,#1843,#1497,.F.);
#2368=EDGE_CURVE('',#1842,#1844,#1498,.T.);
#2369=EDGE_CURVE('',#1845,#1846,#1074,.T.);
#2370=EDGE_CURVE('',#1843,#1845,#1499,.F.);
#2371=EDGE_CURVE('',#1844,#1846,#1500,.T.);
#2372=EDGE_CURVE('',#1847,#1848,#1075,.T.);
#2373=EDGE_CURVE('',#1845,#1847,#1501,.F.);
#2374=EDGE_CURVE('',#1846,#1848,#1502,.T.);
#2375=EDGE_CURVE('',#1849,#1850,#1076,.T.);
#2376=EDGE_CURVE('',#1847,#1849,#1503,.F.);
#2377=EDGE_CURVE('',#1848,#1850,#1504,.T.);
#2378=EDGE_CURVE('',#1851,#1852,#1077,.T.);
#2379=EDGE_CURVE('',#1849,#1851,#1505,.F.);
#2380=EDGE_CURVE('',#1850,#1853,#1506,.T.);
#2381=EDGE_CURVE('',#1853,#1852,#1507,.T.);
#2382=EDGE_CURVE('',#1854,#1855,#1078,.T.);
#2383=EDGE_CURVE('',#1851,#1854,#1508,.F.);
#2384=EDGE_CURVE('',#1852,#1855,#1509,.T.);
#2385=EDGE_CURVE('',#1855,#1856,#1510,.T.);
#2386=EDGE_CURVE('',#1857,#1856,#295,.T.);
#2387=EDGE_CURVE('',#1858,#1857,#1511,.T.);
#2388=EDGE_CURVE('',#1854,#1858,#1512,.T.);
#2389=EDGE_CURVE('',#1859,#1859,#296,.T.);
#2390=EDGE_CURVE('',#1859,#1791,#1079,.T.);
#2391=EDGE_CURVE('',#1825,#1860,#1513,.T.);
#2392=EDGE_CURVE('',#1861,#1860,#297,.F.);
#2393=EDGE_CURVE('',#1861,#1824,#1514,.T.);
#2394=EDGE_CURVE('',#1862,#1862,#298,.T.);
#2395=EDGE_CURVE('',#1863,#1863,#299,.T.);
#2396=EDGE_CURVE('',#1864,#1864,#300,.T.);
#2397=EDGE_CURVE('',#1864,#1865,#301,.T.);
#2398=EDGE_CURVE('',#1865,#1865,#302,.T.);
#2399=EDGE_CURVE('',#1865,#1866,#1080,.T.);
#2400=EDGE_CURVE('',#1866,#1866,#303,.T.);
#2401=EDGE_CURVE('',#1866,#1862,#304,.T.);
#2402=EDGE_CURVE('',#1867,#1867,#305,.T.);
#2403=EDGE_CURVE('',#1860,#1857,#1515,.T.);
#2404=EDGE_CURVE('',#1868,#1789,#1516,.T.);
#2405=EDGE_CURVE('',#1868,#1828,#1517,.T.);
#2406=EDGE_CURVE('',#1786,#1829,#1518,.T.);
#2407=EDGE_CURVE('',#1869,#1861,#1519,.T.);
#2408=EDGE_CURVE('',#1856,#1869,#1520,.T.);
#2409=EDGE_CURVE('',#1870,#1870,#306,.T.);
#2410=EDGE_CURVE('',#1870,#1871,#307,.T.);
#2411=EDGE_CURVE('',#1871,#1871,#308,.T.);
#2412=EDGE_CURVE('',#1871,#1872,#1081,.T.);
#2413=EDGE_CURVE('',#1872,#1872,#309,.T.);
#2414=EDGE_CURVE('',#1873,#1873,#310,.T.);
#2415=EDGE_CURVE('',#1873,#1874,#311,.T.);
#2416=EDGE_CURVE('',#1874,#1874,#312,.T.);
#2417=EDGE_CURVE('',#1874,#1875,#1082,.T.);
#2418=EDGE_CURVE('',#1875,#1875,#313,.T.);
#2419=EDGE_CURVE('',#1875,#1876,#314,.T.);
#2420=EDGE_CURVE('',#1876,#1876,#315,.T.);
#2421=EDGE_CURVE('',#1877,#1877,#316,.T.);
#2422=EDGE_CURVE('',#1878,#1878,#317,.T.);
#2423=EDGE_CURVE('',#1878,#1879,#318,.T.);
#2424=EDGE_CURVE('',#1879,#1879,#319,.T.);
#2425=EDGE_CURVE('',#1879,#1880,#1083,.T.);
#2426=EDGE_CURVE('',#1880,#1880,#320,.T.);
#2427=EDGE_CURVE('',#1881,#1881,#321,.T.);
#2428=EDGE_CURVE('',#1880,#1867,#322,.T.);
#2429=EDGE_CURVE('',#1863,#1882,#323,.T.);
#2430=EDGE_CURVE('',#1882,#1882,#324,.T.);
#2431=EDGE_CURVE('',#1882,#1883,#1084,.T.);
#2432=EDGE_CURVE('',#1883,#1883,#325,.T.);
#2433=EDGE_CURVE('',#1883,#1884,#326,.T.);
#2434=EDGE_CURVE('',#1884,#1884,#327,.T.);
#2435=EDGE_CURVE('',#1885,#1885,#328,.T.);
#2436=EDGE_CURVE('',#1886,#1886,#329,.T.);
#2437=EDGE_CURVE('',#1886,#1887,#330,.T.);
#2438=EDGE_CURVE('',#1887,#1887,#331,.T.);
#2439=EDGE_CURVE('',#1887,#1888,#1085,.T.);
#2440=EDGE_CURVE('',#1888,#1888,#332,.T.);
#2441=EDGE_CURVE('',#1889,#1889,#333,.T.);
#2442=EDGE_CURVE('',#1888,#1890,#334,.T.);
#2443=EDGE_CURVE('',#1890,#1890,#335,.T.);
#2444=EDGE_CURVE('',#1891,#1891,#336,.T.);
#2445=EDGE_CURVE('',#1892,#1892,#337,.T.);
#2446=EDGE_CURVE('',#1892,#1893,#338,.T.);
#2447=EDGE_CURVE('',#1893,#1893,#339,.T.);
#2448=EDGE_CURVE('',#1891,#1892,#1086,.T.);
#2449=EDGE_CURVE('',#1885,#1889,#1087,.T.);
#2450=EDGE_CURVE('',#1877,#1881,#1088,.T.);
#2451=EDGE_CURVE('',#1894,#1894,#340,.T.);
#2452=EDGE_CURVE('',#1894,#1895,#1089,.T.);
#2453=EDGE_CURVE('',#1895,#1895,#341,.T.);
#2454=EDGE_CURVE('',#1896,#1896,#342,.T.);
#2455=EDGE_CURVE('',#1897,#1897,#343,.T.);
#2456=EDGE_CURVE('',#1897,#1896,#1090,.T.);
#2457=ORIENTED_EDGE('',*,*,#1898,.T.);
#2458=ORIENTED_EDGE('',*,*,#1899,.T.);
#2459=ORIENTED_EDGE('',*,*,#1900,.F.);
#2460=ORIENTED_EDGE('',*,*,#1901,.F.);
#2461=ORIENTED_EDGE('',*,*,#1902,.T.);
#2462=ORIENTED_EDGE('',*,*,#1901,.T.);
#2463=ORIENTED_EDGE('',*,*,#1903,.F.);
#2464=ORIENTED_EDGE('',*,*,#1904,.F.);
#2465=ORIENTED_EDGE('',*,*,#1905,.T.);
#2466=ORIENTED_EDGE('',*,*,#1904,.T.);
#2467=ORIENTED_EDGE('',*,*,#1906,.F.);
#2468=ORIENTED_EDGE('',*,*,#1907,.F.);
#2469=ORIENTED_EDGE('',*,*,#1908,.T.);
#2470=ORIENTED_EDGE('',*,*,#1907,.T.);
#2471=ORIENTED_EDGE('',*,*,#1909,.F.);
#2472=ORIENTED_EDGE('',*,*,#1899,.F.);
#2473=ORIENTED_EDGE('',*,*,#1910,.T.);
#2474=ORIENTED_EDGE('',*,*,#1911,.T.);
#2475=ORIENTED_EDGE('',*,*,#1912,.F.);
#2476=ORIENTED_EDGE('',*,*,#1913,.F.);
#2477=ORIENTED_EDGE('',*,*,#1914,.T.);
#2478=ORIENTED_EDGE('',*,*,#1913,.T.);
#2479=ORIENTED_EDGE('',*,*,#1915,.F.);
#2480=ORIENTED_EDGE('',*,*,#1916,.F.);
#2481=ORIENTED_EDGE('',*,*,#1917,.T.);
#2482=ORIENTED_EDGE('',*,*,#1916,.T.);
#2483=ORIENTED_EDGE('',*,*,#1918,.F.);
#2484=ORIENTED_EDGE('',*,*,#1919,.F.);
#2485=ORIENTED_EDGE('',*,*,#1920,.T.);
#2486=ORIENTED_EDGE('',*,*,#1919,.T.);
#2487=ORIENTED_EDGE('',*,*,#1921,.F.);
#2488=ORIENTED_EDGE('',*,*,#1922,.F.);
#2489=ORIENTED_EDGE('',*,*,#1923,.T.);
#2490=ORIENTED_EDGE('',*,*,#1922,.T.);
#2491=ORIENTED_EDGE('',*,*,#1924,.F.);
#2492=ORIENTED_EDGE('',*,*,#1925,.F.);
#2493=ORIENTED_EDGE('',*,*,#1926,.T.);
#2494=ORIENTED_EDGE('',*,*,#1925,.T.);
#2495=ORIENTED_EDGE('',*,*,#1927,.F.);
#2496=ORIENTED_EDGE('',*,*,#1911,.F.);
#2497=ORIENTED_EDGE('',*,*,#1927,.T.);
#2498=ORIENTED_EDGE('',*,*,#1924,.T.);
#2499=ORIENTED_EDGE('',*,*,#1921,.T.);
#2500=ORIENTED_EDGE('',*,*,#1918,.T.);
#2501=ORIENTED_EDGE('',*,*,#1915,.T.);
#2502=ORIENTED_EDGE('',*,*,#1912,.T.);
#2503=ORIENTED_EDGE('',*,*,#1909,.T.);
#2504=ORIENTED_EDGE('',*,*,#1906,.T.);
#2505=ORIENTED_EDGE('',*,*,#1903,.T.);
#2506=ORIENTED_EDGE('',*,*,#1900,.T.);
#2507=ORIENTED_EDGE('',*,*,#1926,.F.);
#2508=ORIENTED_EDGE('',*,*,#1910,.F.);
#2509=ORIENTED_EDGE('',*,*,#1914,.F.);
#2510=ORIENTED_EDGE('',*,*,#1917,.F.);
#2511=ORIENTED_EDGE('',*,*,#1920,.F.);
#2512=ORIENTED_EDGE('',*,*,#1923,.F.);
#2513=ORIENTED_EDGE('',*,*,#1908,.F.);
#2514=ORIENTED_EDGE('',*,*,#1898,.F.);
#2515=ORIENTED_EDGE('',*,*,#1902,.F.);
#2516=ORIENTED_EDGE('',*,*,#1905,.F.);
#2517=ORIENTED_EDGE('',*,*,#1928,.F.);
#2518=ORIENTED_EDGE('',*,*,#1929,.F.);
#2519=ORIENTED_EDGE('',*,*,#1930,.T.);
#2520=ORIENTED_EDGE('',*,*,#1931,.F.);
#2521=ORIENTED_EDGE('',*,*,#1932,.F.);
#2522=ORIENTED_EDGE('',*,*,#1930,.F.);
#2523=ORIENTED_EDGE('',*,*,#1933,.F.);
#2524=ORIENTED_EDGE('',*,*,#1934,.T.);
#2525=ORIENTED_EDGE('',*,*,#1935,.T.);
#2526=ORIENTED_EDGE('',*,*,#1934,.F.);
#2527=ORIENTED_EDGE('',*,*,#1928,.T.);
#2528=ORIENTED_EDGE('',*,*,#1929,.T.);
#2529=ORIENTED_EDGE('',*,*,#1936,.F.);
#2530=ORIENTED_EDGE('',*,*,#1933,.T.);
#2531=ORIENTED_EDGE('',*,*,#1937,.F.);
#2532=ORIENTED_EDGE('',*,*,#1938,.T.);
#2533=ORIENTED_EDGE('',*,*,#1936,.T.);
#2534=ORIENTED_EDGE('',*,*,#1938,.F.);
#2535=ORIENTED_EDGE('',*,*,#1939,.F.);
#2536=ORIENTED_EDGE('',*,*,#1940,.T.);
#2537=ORIENTED_EDGE('',*,*,#1937,.T.);
#2538=ORIENTED_EDGE('',*,*,#1940,.F.);
#2539=ORIENTED_EDGE('',*,*,#1931,.T.);
#2540=ORIENTED_EDGE('',*,*,#1932,.T.);
#2541=ORIENTED_EDGE('',*,*,#1939,.T.);
#2542=ORIENTED_EDGE('',*,*,#1941,.T.);
#2543=ORIENTED_EDGE('',*,*,#1942,.F.);
#2544=ORIENTED_EDGE('',*,*,#1941,.F.);
#2545=ORIENTED_EDGE('',*,*,#1942,.T.);
#2546=ORIENTED_EDGE('',*,*,#1943,.F.);
#2547=ORIENTED_EDGE('',*,*,#1944,.F.);
#2548=ORIENTED_EDGE('',*,*,#1945,.T.);
#2549=ORIENTED_EDGE('',*,*,#1943,.T.);
#2550=ORIENTED_EDGE('',*,*,#1945,.F.);
#2551=ORIENTED_EDGE('',*,*,#1944,.T.);
#2552=ORIENTED_EDGE('',*,*,#1946,.F.);
#2553=ORIENTED_EDGE('',*,*,#1947,.F.);
#2554=ORIENTED_EDGE('',*,*,#1948,.T.);
#2555=ORIENTED_EDGE('',*,*,#1946,.T.);
#2556=ORIENTED_EDGE('',*,*,#1948,.F.);
#2557=ORIENTED_EDGE('',*,*,#1935,.F.);
#2558=ORIENTED_EDGE('',*,*,#1947,.T.);
#2559=ORIENTED_EDGE('',*,*,#1949,.T.);
#2560=ORIENTED_EDGE('',*,*,#1950,.T.);
#2561=ORIENTED_EDGE('',*,*,#1951,.F.);
#2562=ORIENTED_EDGE('',*,*,#1952,.F.);
#2563=ORIENTED_EDGE('',*,*,#1953,.T.);
#2564=ORIENTED_EDGE('',*,*,#1952,.T.);
#2565=ORIENTED_EDGE('',*,*,#1954,.F.);
#2566=ORIENTED_EDGE('',*,*,#1955,.F.);
#2567=ORIENTED_EDGE('',*,*,#1956,.T.);
#2568=ORIENTED_EDGE('',*,*,#1955,.T.);
#2569=ORIENTED_EDGE('',*,*,#1957,.F.);
#2570=ORIENTED_EDGE('',*,*,#1958,.F.);
#2571=ORIENTED_EDGE('',*,*,#1959,.T.);
#2572=ORIENTED_EDGE('',*,*,#1958,.T.);
#2573=ORIENTED_EDGE('',*,*,#1960,.F.);
#2574=ORIENTED_EDGE('',*,*,#1950,.F.);
#2575=ORIENTED_EDGE('',*,*,#1961,.T.);
#2576=ORIENTED_EDGE('',*,*,#1962,.T.);
#2577=ORIENTED_EDGE('',*,*,#1963,.F.);
#2578=ORIENTED_EDGE('',*,*,#1964,.F.);
#2579=ORIENTED_EDGE('',*,*,#1965,.T.);
#2580=ORIENTED_EDGE('',*,*,#1964,.T.);
#2581=ORIENTED_EDGE('',*,*,#1966,.F.);
#2582=ORIENTED_EDGE('',*,*,#1967,.F.);
#2583=ORIENTED_EDGE('',*,*,#1968,.T.);
#2584=ORIENTED_EDGE('',*,*,#1967,.T.);
#2585=ORIENTED_EDGE('',*,*,#1969,.F.);
#2586=ORIENTED_EDGE('',*,*,#1970,.F.);
#2587=ORIENTED_EDGE('',*,*,#1971,.T.);
#2588=ORIENTED_EDGE('',*,*,#1970,.T.);
#2589=ORIENTED_EDGE('',*,*,#1972,.F.);
#2590=ORIENTED_EDGE('',*,*,#1973,.F.);
#2591=ORIENTED_EDGE('',*,*,#1974,.T.);
#2592=ORIENTED_EDGE('',*,*,#1973,.T.);
#2593=ORIENTED_EDGE('',*,*,#1975,.F.);
#2594=ORIENTED_EDGE('',*,*,#1976,.F.);
#2595=ORIENTED_EDGE('',*,*,#1977,.T.);
#2596=ORIENTED_EDGE('',*,*,#1976,.T.);
#2597=ORIENTED_EDGE('',*,*,#1978,.F.);
#2598=ORIENTED_EDGE('',*,*,#1962,.F.);
#2599=ORIENTED_EDGE('',*,*,#1978,.T.);
#2600=ORIENTED_EDGE('',*,*,#1975,.T.);
#2601=ORIENTED_EDGE('',*,*,#1972,.T.);
#2602=ORIENTED_EDGE('',*,*,#1969,.T.);
#2603=ORIENTED_EDGE('',*,*,#1966,.T.);
#2604=ORIENTED_EDGE('',*,*,#1963,.T.);
#2605=ORIENTED_EDGE('',*,*,#1960,.T.);
#2606=ORIENTED_EDGE('',*,*,#1957,.T.);
#2607=ORIENTED_EDGE('',*,*,#1954,.T.);
#2608=ORIENTED_EDGE('',*,*,#1951,.T.);
#2609=ORIENTED_EDGE('',*,*,#1977,.F.);
#2610=ORIENTED_EDGE('',*,*,#1961,.F.);
#2611=ORIENTED_EDGE('',*,*,#1965,.F.);
#2612=ORIENTED_EDGE('',*,*,#1968,.F.);
#2613=ORIENTED_EDGE('',*,*,#1971,.F.);
#2614=ORIENTED_EDGE('',*,*,#1974,.F.);
#2615=ORIENTED_EDGE('',*,*,#1959,.F.);
#2616=ORIENTED_EDGE('',*,*,#1949,.F.);
#2617=ORIENTED_EDGE('',*,*,#1953,.F.);
#2618=ORIENTED_EDGE('',*,*,#1956,.F.);
#2619=ORIENTED_EDGE('',*,*,#1979,.F.);
#2620=ORIENTED_EDGE('',*,*,#1980,.T.);
#2621=ORIENTED_EDGE('',*,*,#1981,.F.);
#2622=ORIENTED_EDGE('',*,*,#1982,.F.);
#2623=ORIENTED_EDGE('',*,*,#1983,.F.);
#2624=ORIENTED_EDGE('',*,*,#1984,.F.);
#2625=ORIENTED_EDGE('',*,*,#1985,.F.);
#2626=ORIENTED_EDGE('',*,*,#1986,.F.);
#2627=ORIENTED_EDGE('',*,*,#1987,.F.);
#2628=ORIENTED_EDGE('',*,*,#1988,.F.);
#2629=ORIENTED_EDGE('',*,*,#1989,.F.);
#2630=ORIENTED_EDGE('',*,*,#1990,.F.);
#2631=ORIENTED_EDGE('',*,*,#1991,.F.);
#2632=ORIENTED_EDGE('',*,*,#1992,.F.);
#2633=ORIENTED_EDGE('',*,*,#1993,.F.);
#2634=ORIENTED_EDGE('',*,*,#1994,.F.);
#2635=ORIENTED_EDGE('',*,*,#1995,.F.);
#2636=ORIENTED_EDGE('',*,*,#1996,.F.);
#2637=ORIENTED_EDGE('',*,*,#1997,.F.);
#2638=ORIENTED_EDGE('',*,*,#1998,.F.);
#2639=ORIENTED_EDGE('',*,*,#1999,.F.);
#2640=ORIENTED_EDGE('',*,*,#2000,.F.);
#2641=ORIENTED_EDGE('',*,*,#2001,.F.);
#2642=ORIENTED_EDGE('',*,*,#2002,.F.);
#2643=ORIENTED_EDGE('',*,*,#2003,.F.);
#2644=ORIENTED_EDGE('',*,*,#2004,.F.);
#2645=ORIENTED_EDGE('',*,*,#2005,.F.);
#2646=ORIENTED_EDGE('',*,*,#2006,.F.);
#2647=ORIENTED_EDGE('',*,*,#2007,.F.);
#2648=ORIENTED_EDGE('',*,*,#2008,.F.);
#2649=ORIENTED_EDGE('',*,*,#2009,.F.);
#2650=ORIENTED_EDGE('',*,*,#2010,.F.);
#2651=ORIENTED_EDGE('',*,*,#2011,.F.);
#2652=ORIENTED_EDGE('',*,*,#2012,.F.);
#2653=ORIENTED_EDGE('',*,*,#2013,.F.);
#2654=ORIENTED_EDGE('',*,*,#2014,.F.);
#2655=ORIENTED_EDGE('',*,*,#2015,.F.);
#2656=ORIENTED_EDGE('',*,*,#2016,.F.);
#2657=ORIENTED_EDGE('',*,*,#2017,.F.);
#2658=ORIENTED_EDGE('',*,*,#2018,.F.);
#2659=ORIENTED_EDGE('',*,*,#2019,.F.);
#2660=ORIENTED_EDGE('',*,*,#2020,.F.);
#2661=ORIENTED_EDGE('',*,*,#2021,.F.);
#2662=ORIENTED_EDGE('',*,*,#2022,.F.);
#2663=ORIENTED_EDGE('',*,*,#2023,.F.);
#2664=ORIENTED_EDGE('',*,*,#2024,.F.);
#2665=ORIENTED_EDGE('',*,*,#2025,.F.);
#2666=ORIENTED_EDGE('',*,*,#2026,.F.);
#2667=ORIENTED_EDGE('',*,*,#2027,.F.);
#2668=ORIENTED_EDGE('',*,*,#2028,.F.);
#2669=ORIENTED_EDGE('',*,*,#2029,.F.);
#2670=ORIENTED_EDGE('',*,*,#2030,.F.);
#2671=ORIENTED_EDGE('',*,*,#2031,.F.);
#2672=ORIENTED_EDGE('',*,*,#2032,.F.);
#2673=ORIENTED_EDGE('',*,*,#2033,.F.);
#2674=ORIENTED_EDGE('',*,*,#2034,.F.);
#2675=ORIENTED_EDGE('',*,*,#2035,.F.);
#2676=ORIENTED_EDGE('',*,*,#2036,.F.);
#2677=ORIENTED_EDGE('',*,*,#2037,.F.);
#2678=ORIENTED_EDGE('',*,*,#2038,.F.);
#2679=ORIENTED_EDGE('',*,*,#2039,.F.);
#2680=ORIENTED_EDGE('',*,*,#2040,.F.);
#2681=ORIENTED_EDGE('',*,*,#2041,.F.);
#2682=ORIENTED_EDGE('',*,*,#2042,.F.);
#2683=ORIENTED_EDGE('',*,*,#2043,.F.);
#2684=ORIENTED_EDGE('',*,*,#2044,.F.);
#2685=ORIENTED_EDGE('',*,*,#2045,.F.);
#2686=ORIENTED_EDGE('',*,*,#2046,.F.);
#2687=ORIENTED_EDGE('',*,*,#2047,.F.);
#2688=ORIENTED_EDGE('',*,*,#2048,.F.);
#2689=ORIENTED_EDGE('',*,*,#2049,.F.);
#2690=ORIENTED_EDGE('',*,*,#2050,.F.);
#2691=ORIENTED_EDGE('',*,*,#2051,.F.);
#2692=ORIENTED_EDGE('',*,*,#2052,.F.);
#2693=ORIENTED_EDGE('',*,*,#2053,.F.);
#2694=ORIENTED_EDGE('',*,*,#2054,.F.);
#2695=ORIENTED_EDGE('',*,*,#2055,.F.);
#2696=ORIENTED_EDGE('',*,*,#2056,.F.);
#2697=ORIENTED_EDGE('',*,*,#2057,.F.);
#2698=ORIENTED_EDGE('',*,*,#2058,.F.);
#2699=ORIENTED_EDGE('',*,*,#2059,.F.);
#2700=ORIENTED_EDGE('',*,*,#2060,.F.);
#2701=ORIENTED_EDGE('',*,*,#2061,.F.);
#2702=ORIENTED_EDGE('',*,*,#2062,.F.);
#2703=ORIENTED_EDGE('',*,*,#2063,.F.);
#2704=ORIENTED_EDGE('',*,*,#2064,.F.);
#2705=ORIENTED_EDGE('',*,*,#2065,.F.);
#2706=ORIENTED_EDGE('',*,*,#2066,.F.);
#2707=ORIENTED_EDGE('',*,*,#2067,.F.);
#2708=ORIENTED_EDGE('',*,*,#2068,.F.);
#2709=ORIENTED_EDGE('',*,*,#2069,.F.);
#2710=ORIENTED_EDGE('',*,*,#2070,.F.);
#2711=ORIENTED_EDGE('',*,*,#2071,.F.);
#2712=ORIENTED_EDGE('',*,*,#2072,.F.);
#2713=ORIENTED_EDGE('',*,*,#2073,.F.);
#2714=ORIENTED_EDGE('',*,*,#2074,.F.);
#2715=ORIENTED_EDGE('',*,*,#2075,.F.);
#2716=ORIENTED_EDGE('',*,*,#2076,.F.);
#2717=ORIENTED_EDGE('',*,*,#2077,.F.);
#2718=ORIENTED_EDGE('',*,*,#2078,.F.);
#2719=ORIENTED_EDGE('',*,*,#2079,.F.);
#2720=ORIENTED_EDGE('',*,*,#2080,.F.);
#2721=ORIENTED_EDGE('',*,*,#2081,.F.);
#2722=ORIENTED_EDGE('',*,*,#2082,.F.);
#2723=ORIENTED_EDGE('',*,*,#2083,.F.);
#2724=ORIENTED_EDGE('',*,*,#2084,.F.);
#2725=ORIENTED_EDGE('',*,*,#2085,.F.);
#2726=ORIENTED_EDGE('',*,*,#2086,.F.);
#2727=ORIENTED_EDGE('',*,*,#2087,.F.);
#2728=ORIENTED_EDGE('',*,*,#2088,.T.);
#2729=ORIENTED_EDGE('',*,*,#2006,.T.);
#2730=ORIENTED_EDGE('',*,*,#2089,.T.);
#2731=ORIENTED_EDGE('',*,*,#2090,.F.);
#2732=ORIENTED_EDGE('',*,*,#2009,.T.);
#2733=ORIENTED_EDGE('',*,*,#2091,.F.);
#2734=ORIENTED_EDGE('',*,*,#2057,.T.);
#2735=ORIENTED_EDGE('',*,*,#2092,.T.);
#2736=ORIENTED_EDGE('',*,*,#2002,.T.);
#2737=ORIENTED_EDGE('',*,*,#2093,.T.);
#2738=ORIENTED_EDGE('',*,*,#2064,.T.);
#2739=ORIENTED_EDGE('',*,*,#2094,.F.);
#2740=ORIENTED_EDGE('',*,*,#2013,.T.);
#2741=ORIENTED_EDGE('',*,*,#2095,.F.);
#2742=ORIENTED_EDGE('',*,*,#2053,.T.);
#2743=ORIENTED_EDGE('',*,*,#2096,.T.);
#2744=ORIENTED_EDGE('',*,*,#1998,.T.);
#2745=ORIENTED_EDGE('',*,*,#2097,.T.);
#2746=ORIENTED_EDGE('',*,*,#2068,.T.);
#2747=ORIENTED_EDGE('',*,*,#2098,.F.);
#2748=ORIENTED_EDGE('',*,*,#2017,.T.);
#2749=ORIENTED_EDGE('',*,*,#2099,.F.);
#2750=ORIENTED_EDGE('',*,*,#2049,.T.);
#2751=ORIENTED_EDGE('',*,*,#2100,.T.);
#2752=ORIENTED_EDGE('',*,*,#1994,.T.);
#2753=ORIENTED_EDGE('',*,*,#2101,.T.);
#2754=ORIENTED_EDGE('',*,*,#2072,.T.);
#2755=ORIENTED_EDGE('',*,*,#2102,.F.);
#2756=ORIENTED_EDGE('',*,*,#2021,.T.);
#2757=ORIENTED_EDGE('',*,*,#2103,.F.);
#2758=ORIENTED_EDGE('',*,*,#2045,.T.);
#2759=ORIENTED_EDGE('',*,*,#2104,.T.);
#2760=ORIENTED_EDGE('',*,*,#1990,.T.);
#2761=ORIENTED_EDGE('',*,*,#2105,.T.);
#2762=ORIENTED_EDGE('',*,*,#2076,.T.);
#2763=ORIENTED_EDGE('',*,*,#2106,.F.);
#2764=ORIENTED_EDGE('',*,*,#2025,.T.);
#2765=ORIENTED_EDGE('',*,*,#2107,.F.);
#2766=ORIENTED_EDGE('',*,*,#2041,.T.);
#2767=ORIENTED_EDGE('',*,*,#2108,.T.);
#2768=ORIENTED_EDGE('',*,*,#1986,.T.);
#2769=ORIENTED_EDGE('',*,*,#2109,.T.);
#2770=ORIENTED_EDGE('',*,*,#2080,.T.);
#2771=ORIENTED_EDGE('',*,*,#2110,.F.);
#2772=ORIENTED_EDGE('',*,*,#2029,.T.);
#2773=ORIENTED_EDGE('',*,*,#2111,.F.);
#2774=ORIENTED_EDGE('',*,*,#2037,.T.);
#2775=ORIENTED_EDGE('',*,*,#2112,.T.);
#2776=ORIENTED_EDGE('',*,*,#1982,.T.);
#2777=ORIENTED_EDGE('',*,*,#2113,.T.);
#2778=ORIENTED_EDGE('',*,*,#2084,.T.);
#2779=ORIENTED_EDGE('',*,*,#2114,.F.);
#2780=ORIENTED_EDGE('',*,*,#2033,.T.);
#2781=ORIENTED_EDGE('',*,*,#2115,.F.);
#2782=ORIENTED_EDGE('',*,*,#2116,.F.);
#2783=ORIENTED_EDGE('',*,*,#2117,.T.);
#2784=ORIENTED_EDGE('',*,*,#2087,.T.);
#2785=ORIENTED_EDGE('',*,*,#2118,.F.);
#2786=ORIENTED_EDGE('',*,*,#2119,.F.);
#2787=ORIENTED_EDGE('',*,*,#2008,.T.);
#2788=ORIENTED_EDGE('',*,*,#2120,.F.);
#2789=ORIENTED_EDGE('',*,*,#2121,.F.);
#2790=ORIENTED_EDGE('',*,*,#2058,.T.);
#2791=ORIENTED_EDGE('',*,*,#2091,.T.);
#2792=ORIENTED_EDGE('',*,*,#2012,.T.);
#2793=ORIENTED_EDGE('',*,*,#2122,.F.);
#2794=ORIENTED_EDGE('',*,*,#2054,.T.);
#2795=ORIENTED_EDGE('',*,*,#2095,.T.);
#2796=ORIENTED_EDGE('',*,*,#2016,.T.);
#2797=ORIENTED_EDGE('',*,*,#2123,.F.);
#2798=ORIENTED_EDGE('',*,*,#2050,.T.);
#2799=ORIENTED_EDGE('',*,*,#2099,.T.);
#2800=ORIENTED_EDGE('',*,*,#2020,.T.);
#2801=ORIENTED_EDGE('',*,*,#2124,.F.);
#2802=ORIENTED_EDGE('',*,*,#2046,.T.);
#2803=ORIENTED_EDGE('',*,*,#2103,.T.);
#2804=ORIENTED_EDGE('',*,*,#2024,.T.);
#2805=ORIENTED_EDGE('',*,*,#2125,.F.);
#2806=ORIENTED_EDGE('',*,*,#2042,.T.);
#2807=ORIENTED_EDGE('',*,*,#2107,.T.);
#2808=ORIENTED_EDGE('',*,*,#2028,.T.);
#2809=ORIENTED_EDGE('',*,*,#2126,.F.);
#2810=ORIENTED_EDGE('',*,*,#2038,.T.);
#2811=ORIENTED_EDGE('',*,*,#2111,.T.);
#2812=ORIENTED_EDGE('',*,*,#2032,.T.);
#2813=ORIENTED_EDGE('',*,*,#2127,.F.);
#2814=ORIENTED_EDGE('',*,*,#2034,.T.);
#2815=ORIENTED_EDGE('',*,*,#2128,.F.);
#2816=ORIENTED_EDGE('',*,*,#2115,.T.);
#2817=ORIENTED_EDGE('',*,*,#2003,.T.);
#2818=ORIENTED_EDGE('',*,*,#2094,.T.);
#2819=ORIENTED_EDGE('',*,*,#2063,.T.);
#2820=ORIENTED_EDGE('',*,*,#2129,.F.);
#2821=ORIENTED_EDGE('',*,*,#1999,.T.);
#2822=ORIENTED_EDGE('',*,*,#2098,.T.);
#2823=ORIENTED_EDGE('',*,*,#2067,.T.);
#2824=ORIENTED_EDGE('',*,*,#2130,.F.);
#2825=ORIENTED_EDGE('',*,*,#1995,.T.);
#2826=ORIENTED_EDGE('',*,*,#2102,.T.);
#2827=ORIENTED_EDGE('',*,*,#2071,.T.);
#2828=ORIENTED_EDGE('',*,*,#2131,.F.);
#2829=ORIENTED_EDGE('',*,*,#1991,.T.);
#2830=ORIENTED_EDGE('',*,*,#2106,.T.);
#2831=ORIENTED_EDGE('',*,*,#2075,.T.);
#2832=ORIENTED_EDGE('',*,*,#2132,.F.);
#2833=ORIENTED_EDGE('',*,*,#1987,.T.);
#2834=ORIENTED_EDGE('',*,*,#2110,.T.);
#2835=ORIENTED_EDGE('',*,*,#2079,.T.);
#2836=ORIENTED_EDGE('',*,*,#2133,.F.);
#2837=ORIENTED_EDGE('',*,*,#1983,.T.);
#2838=ORIENTED_EDGE('',*,*,#2114,.T.);
#2839=ORIENTED_EDGE('',*,*,#2083,.T.);
#2840=ORIENTED_EDGE('',*,*,#2134,.F.);
#2841=ORIENTED_EDGE('',*,*,#2007,.T.);
#2842=ORIENTED_EDGE('',*,*,#2090,.T.);
#2843=ORIENTED_EDGE('',*,*,#2135,.T.);
#2844=ORIENTED_EDGE('',*,*,#2060,.T.);
#2845=ORIENTED_EDGE('',*,*,#2136,.T.);
#2846=ORIENTED_EDGE('',*,*,#2120,.T.);
#2847=ORIENTED_EDGE('',*,*,#2059,.T.);
#2848=ORIENTED_EDGE('',*,*,#2121,.T.);
#2849=ORIENTED_EDGE('',*,*,#2136,.F.);
#2850=ORIENTED_EDGE('',*,*,#2086,.T.);
#2851=ORIENTED_EDGE('',*,*,#2137,.T.);
#2852=ORIENTED_EDGE('',*,*,#2138,.F.);
#2853=ORIENTED_EDGE('',*,*,#2118,.T.);
#2854=ORIENTED_EDGE('',*,*,#2004,.T.);
#2855=ORIENTED_EDGE('',*,*,#2129,.T.);
#2856=ORIENTED_EDGE('',*,*,#2062,.T.);
#2857=ORIENTED_EDGE('',*,*,#2139,.T.);
#2858=ORIENTED_EDGE('',*,*,#2011,.T.);
#2859=ORIENTED_EDGE('',*,*,#2140,.T.);
#2860=ORIENTED_EDGE('',*,*,#2055,.T.);
#2861=ORIENTED_EDGE('',*,*,#2122,.T.);
#2862=ORIENTED_EDGE('',*,*,#2000,.T.);
#2863=ORIENTED_EDGE('',*,*,#2130,.T.);
#2864=ORIENTED_EDGE('',*,*,#2066,.T.);
#2865=ORIENTED_EDGE('',*,*,#2141,.T.);
#2866=ORIENTED_EDGE('',*,*,#2015,.T.);
#2867=ORIENTED_EDGE('',*,*,#2142,.T.);
#2868=ORIENTED_EDGE('',*,*,#2051,.T.);
#2869=ORIENTED_EDGE('',*,*,#2123,.T.);
#2870=ORIENTED_EDGE('',*,*,#1996,.T.);
#2871=ORIENTED_EDGE('',*,*,#2131,.T.);
#2872=ORIENTED_EDGE('',*,*,#2070,.T.);
#2873=ORIENTED_EDGE('',*,*,#2143,.T.);
#2874=ORIENTED_EDGE('',*,*,#2019,.T.);
#2875=ORIENTED_EDGE('',*,*,#2144,.T.);
#2876=ORIENTED_EDGE('',*,*,#2047,.T.);
#2877=ORIENTED_EDGE('',*,*,#2124,.T.);
#2878=ORIENTED_EDGE('',*,*,#1992,.T.);
#2879=ORIENTED_EDGE('',*,*,#2132,.T.);
#2880=ORIENTED_EDGE('',*,*,#2074,.T.);
#2881=ORIENTED_EDGE('',*,*,#2145,.T.);
#2882=ORIENTED_EDGE('',*,*,#2023,.T.);
#2883=ORIENTED_EDGE('',*,*,#2146,.T.);
#2884=ORIENTED_EDGE('',*,*,#2043,.T.);
#2885=ORIENTED_EDGE('',*,*,#2125,.T.);
#2886=ORIENTED_EDGE('',*,*,#1988,.T.);
#2887=ORIENTED_EDGE('',*,*,#2133,.T.);
#2888=ORIENTED_EDGE('',*,*,#2078,.T.);
#2889=ORIENTED_EDGE('',*,*,#2147,.T.);
#2890=ORIENTED_EDGE('',*,*,#2027,.T.);
#2891=ORIENTED_EDGE('',*,*,#2148,.T.);
#2892=ORIENTED_EDGE('',*,*,#2039,.T.);
#2893=ORIENTED_EDGE('',*,*,#2126,.T.);
#2894=ORIENTED_EDGE('',*,*,#1984,.T.);
#2895=ORIENTED_EDGE('',*,*,#2134,.T.);
#2896=ORIENTED_EDGE('',*,*,#2082,.T.);
#2897=ORIENTED_EDGE('',*,*,#2149,.T.);
#2898=ORIENTED_EDGE('',*,*,#2031,.T.);
#2899=ORIENTED_EDGE('',*,*,#2150,.T.);
#2900=ORIENTED_EDGE('',*,*,#2035,.T.);
#2901=ORIENTED_EDGE('',*,*,#2127,.T.);
#2902=ORIENTED_EDGE('',*,*,#2010,.T.);
#2903=ORIENTED_EDGE('',*,*,#2092,.F.);
#2904=ORIENTED_EDGE('',*,*,#2056,.T.);
#2905=ORIENTED_EDGE('',*,*,#2140,.F.);
#2906=ORIENTED_EDGE('',*,*,#2014,.T.);
#2907=ORIENTED_EDGE('',*,*,#2096,.F.);
#2908=ORIENTED_EDGE('',*,*,#2052,.T.);
#2909=ORIENTED_EDGE('',*,*,#2142,.F.);
#2910=ORIENTED_EDGE('',*,*,#2018,.T.);
#2911=ORIENTED_EDGE('',*,*,#2100,.F.);
#2912=ORIENTED_EDGE('',*,*,#2048,.T.);
#2913=ORIENTED_EDGE('',*,*,#2144,.F.);
#2914=ORIENTED_EDGE('',*,*,#2022,.T.);
#2915=ORIENTED_EDGE('',*,*,#2104,.F.);
#2916=ORIENTED_EDGE('',*,*,#2044,.T.);
#2917=ORIENTED_EDGE('',*,*,#2146,.F.);
#2918=ORIENTED_EDGE('',*,*,#2026,.T.);
#2919=ORIENTED_EDGE('',*,*,#2108,.F.);
#2920=ORIENTED_EDGE('',*,*,#2040,.T.);
#2921=ORIENTED_EDGE('',*,*,#2148,.F.);
#2922=ORIENTED_EDGE('',*,*,#2030,.T.);
#2923=ORIENTED_EDGE('',*,*,#2112,.F.);
#2924=ORIENTED_EDGE('',*,*,#2036,.T.);
#2925=ORIENTED_EDGE('',*,*,#2150,.F.);
#2926=ORIENTED_EDGE('',*,*,#2005,.T.);
#2927=ORIENTED_EDGE('',*,*,#2139,.F.);
#2928=ORIENTED_EDGE('',*,*,#2061,.T.);
#2929=ORIENTED_EDGE('',*,*,#2135,.F.);
#2930=ORIENTED_EDGE('',*,*,#2089,.F.);
#2931=ORIENTED_EDGE('',*,*,#2001,.T.);
#2932=ORIENTED_EDGE('',*,*,#2141,.F.);
#2933=ORIENTED_EDGE('',*,*,#2065,.T.);
#2934=ORIENTED_EDGE('',*,*,#2093,.F.);
#2935=ORIENTED_EDGE('',*,*,#1997,.T.);
#2936=ORIENTED_EDGE('',*,*,#2143,.F.);
#2937=ORIENTED_EDGE('',*,*,#2069,.T.);
#2938=ORIENTED_EDGE('',*,*,#2097,.F.);
#2939=ORIENTED_EDGE('',*,*,#1993,.T.);
#2940=ORIENTED_EDGE('',*,*,#2145,.F.);
#2941=ORIENTED_EDGE('',*,*,#2073,.T.);
#2942=ORIENTED_EDGE('',*,*,#2101,.F.);
#2943=ORIENTED_EDGE('',*,*,#1989,.T.);
#2944=ORIENTED_EDGE('',*,*,#2147,.F.);
#2945=ORIENTED_EDGE('',*,*,#2077,.T.);
#2946=ORIENTED_EDGE('',*,*,#2105,.F.);
#2947=ORIENTED_EDGE('',*,*,#1985,.T.);
#2948=ORIENTED_EDGE('',*,*,#2149,.F.);
#2949=ORIENTED_EDGE('',*,*,#2081,.T.);
#2950=ORIENTED_EDGE('',*,*,#2109,.F.);
#2951=ORIENTED_EDGE('',*,*,#1981,.T.);
#2952=ORIENTED_EDGE('',*,*,#2151,.F.);
#2953=ORIENTED_EDGE('',*,*,#2137,.F.);
#2954=ORIENTED_EDGE('',*,*,#2085,.T.);
#2955=ORIENTED_EDGE('',*,*,#2113,.F.);
#2956=ORIENTED_EDGE('',*,*,#1979,.T.);
#2957=ORIENTED_EDGE('',*,*,#2117,.F.);
#2958=ORIENTED_EDGE('',*,*,#2152,.F.);
#2959=ORIENTED_EDGE('',*,*,#2153,.F.);
#2960=ORIENTED_EDGE('',*,*,#2154,.T.);
#2961=ORIENTED_EDGE('',*,*,#2155,.F.);
#2962=ORIENTED_EDGE('',*,*,#2154,.F.);
#2963=ORIENTED_EDGE('',*,*,#2155,.T.);
#2964=ORIENTED_EDGE('',*,*,#2152,.T.);
#2965=ORIENTED_EDGE('',*,*,#2116,.T.);
#2966=ORIENTED_EDGE('',*,*,#2128,.T.);
#2967=ORIENTED_EDGE('',*,*,#2088,.F.);
#2968=ORIENTED_EDGE('',*,*,#2119,.T.);
#2969=ORIENTED_EDGE('',*,*,#2138,.T.);
#2970=ORIENTED_EDGE('',*,*,#2151,.T.);
#2971=ORIENTED_EDGE('',*,*,#1980,.F.);
#2972=ORIENTED_EDGE('',*,*,#2153,.T.);
#2973=ORIENTED_EDGE('',*,*,#2156,.T.);
#2974=ORIENTED_EDGE('',*,*,#2157,.T.);
#2975=ORIENTED_EDGE('',*,*,#2158,.T.);
#2976=ORIENTED_EDGE('',*,*,#2157,.F.);
#2977=ORIENTED_EDGE('',*,*,#2158,.F.);
#2978=ORIENTED_EDGE('',*,*,#2159,.T.);
#2979=ORIENTED_EDGE('',*,*,#2160,.F.);
#2980=ORIENTED_EDGE('',*,*,#2159,.F.);
#2981=ORIENTED_EDGE('',*,*,#2156,.F.);
#2982=ORIENTED_EDGE('',*,*,#2160,.T.);
#2983=ORIENTED_EDGE('',*,*,#2161,.T.);
#2984=ORIENTED_EDGE('',*,*,#2162,.T.);
#2985=ORIENTED_EDGE('',*,*,#2161,.F.);
#2986=ORIENTED_EDGE('',*,*,#2162,.F.);
#2987=ORIENTED_EDGE('',*,*,#2163,.F.);
#2988=ORIENTED_EDGE('',*,*,#2164,.F.);
#2989=ORIENTED_EDGE('',*,*,#2165,.F.);
#2990=ORIENTED_EDGE('',*,*,#2166,.T.);
#2991=ORIENTED_EDGE('',*,*,#2167,.F.);
#2992=ORIENTED_EDGE('',*,*,#2168,.F.);
#2993=ORIENTED_EDGE('',*,*,#2163,.T.);
#2994=ORIENTED_EDGE('',*,*,#2169,.T.);
#2995=ORIENTED_EDGE('',*,*,#2170,.F.);
#2996=ORIENTED_EDGE('',*,*,#2171,.F.);
#2997=ORIENTED_EDGE('',*,*,#2167,.T.);
#2998=ORIENTED_EDGE('',*,*,#2172,.T.);
#2999=ORIENTED_EDGE('',*,*,#2173,.F.);
#3000=ORIENTED_EDGE('',*,*,#2174,.F.);
#3001=ORIENTED_EDGE('',*,*,#2170,.T.);
#3002=ORIENTED_EDGE('',*,*,#2175,.T.);
#3003=ORIENTED_EDGE('',*,*,#2176,.F.);
#3004=ORIENTED_EDGE('',*,*,#2177,.F.);
#3005=ORIENTED_EDGE('',*,*,#2173,.T.);
#3006=ORIENTED_EDGE('',*,*,#2178,.T.);
#3007=ORIENTED_EDGE('',*,*,#2179,.F.);
#3008=ORIENTED_EDGE('',*,*,#2180,.F.);
#3009=ORIENTED_EDGE('',*,*,#2176,.T.);
#3010=ORIENTED_EDGE('',*,*,#2181,.T.);
#3011=ORIENTED_EDGE('',*,*,#2179,.T.);
#3012=ORIENTED_EDGE('',*,*,#2182,.T.);
#3013=ORIENTED_EDGE('',*,*,#2183,.T.);
#3014=ORIENTED_EDGE('',*,*,#2184,.F.);
#3015=ORIENTED_EDGE('',*,*,#2185,.F.);
#3016=ORIENTED_EDGE('',*,*,#2186,.F.);
#3017=ORIENTED_EDGE('',*,*,#2187,.T.);
#3018=ORIENTED_EDGE('',*,*,#2188,.T.);
#3019=ORIENTED_EDGE('',*,*,#2189,.T.);
#3020=ORIENTED_EDGE('',*,*,#2190,.T.);
#3021=ORIENTED_EDGE('',*,*,#2191,.T.);
#3022=ORIENTED_EDGE('',*,*,#2192,.T.);
#3023=ORIENTED_EDGE('',*,*,#2193,.T.);
#3024=ORIENTED_EDGE('',*,*,#2194,.T.);
#3025=ORIENTED_EDGE('',*,*,#2195,.T.);
#3026=ORIENTED_EDGE('',*,*,#2196,.T.);
#3027=ORIENTED_EDGE('',*,*,#2197,.F.);
#3028=ORIENTED_EDGE('',*,*,#2198,.T.);
#3029=ORIENTED_EDGE('',*,*,#2199,.T.);
#3030=ORIENTED_EDGE('',*,*,#2200,.T.);
#3031=ORIENTED_EDGE('',*,*,#2201,.T.);
#3032=ORIENTED_EDGE('',*,*,#2202,.T.);
#3033=ORIENTED_EDGE('',*,*,#2203,.T.);
#3034=ORIENTED_EDGE('',*,*,#2204,.T.);
#3035=ORIENTED_EDGE('',*,*,#2205,.F.);
#3036=ORIENTED_EDGE('',*,*,#2206,.T.);
#3037=ORIENTED_EDGE('',*,*,#2207,.T.);
#3038=ORIENTED_EDGE('',*,*,#2208,.T.);
#3039=ORIENTED_EDGE('',*,*,#2209,.F.);
#3040=ORIENTED_EDGE('',*,*,#2210,.T.);
#3041=ORIENTED_EDGE('',*,*,#2211,.T.);
#3042=ORIENTED_EDGE('',*,*,#2212,.F.);
#3043=ORIENTED_EDGE('',*,*,#2208,.F.);
#3044=ORIENTED_EDGE('',*,*,#2213,.F.);
#3045=ORIENTED_EDGE('',*,*,#2211,.F.);
#3046=ORIENTED_EDGE('',*,*,#2214,.T.);
#3047=ORIENTED_EDGE('',*,*,#2215,.T.);
#3048=ORIENTED_EDGE('',*,*,#2216,.T.);
#3049=ORIENTED_EDGE('',*,*,#2217,.T.);
#3050=ORIENTED_EDGE('',*,*,#2218,.T.);
#3051=ORIENTED_EDGE('',*,*,#2215,.F.);
#3052=ORIENTED_EDGE('',*,*,#2214,.F.);
#3053=ORIENTED_EDGE('',*,*,#2210,.F.);
#3054=ORIENTED_EDGE('',*,*,#2207,.F.);
#3055=ORIENTED_EDGE('',*,*,#2219,.F.);
#3056=ORIENTED_EDGE('',*,*,#2220,.T.);
#3057=ORIENTED_EDGE('',*,*,#2217,.F.);
#3058=ORIENTED_EDGE('',*,*,#2206,.F.);
#3059=ORIENTED_EDGE('',*,*,#2221,.F.);
#3060=ORIENTED_EDGE('',*,*,#2216,.F.);
#3061=ORIENTED_EDGE('',*,*,#2218,.F.);
#3062=ORIENTED_EDGE('',*,*,#2220,.F.);
#3063=ORIENTED_EDGE('',*,*,#2222,.F.);
#3064=ORIENTED_EDGE('',*,*,#2196,.F.);
#3065=ORIENTED_EDGE('',*,*,#2195,.F.);
#3066=ORIENTED_EDGE('',*,*,#2194,.F.);
#3067=ORIENTED_EDGE('',*,*,#2193,.F.);
#3068=ORIENTED_EDGE('',*,*,#2192,.F.);
#3069=ORIENTED_EDGE('',*,*,#2191,.F.);
#3070=ORIENTED_EDGE('',*,*,#2190,.F.);
#3071=ORIENTED_EDGE('',*,*,#2189,.F.);
#3072=ORIENTED_EDGE('',*,*,#2223,.F.);
#3073=ORIENTED_EDGE('',*,*,#2224,.T.);
#3074=ORIENTED_EDGE('',*,*,#2164,.T.);
#3075=ORIENTED_EDGE('',*,*,#2168,.T.);
#3076=ORIENTED_EDGE('',*,*,#2171,.T.);
#3077=ORIENTED_EDGE('',*,*,#2174,.T.);
#3078=ORIENTED_EDGE('',*,*,#2177,.T.);
#3079=ORIENTED_EDGE('',*,*,#2180,.T.);
#3080=ORIENTED_EDGE('',*,*,#2186,.T.);
#3081=ORIENTED_EDGE('',*,*,#2185,.T.);
#3082=ORIENTED_EDGE('',*,*,#2225,.F.);
#3083=ORIENTED_EDGE('',*,*,#2226,.F.);
#3084=ORIENTED_EDGE('',*,*,#2183,.F.);
#3085=ORIENTED_EDGE('',*,*,#2182,.F.);
#3086=ORIENTED_EDGE('',*,*,#2181,.F.);
#3087=ORIENTED_EDGE('',*,*,#2178,.F.);
#3088=ORIENTED_EDGE('',*,*,#2175,.F.);
#3089=ORIENTED_EDGE('',*,*,#2172,.F.);
#3090=ORIENTED_EDGE('',*,*,#2169,.F.);
#3091=ORIENTED_EDGE('',*,*,#2166,.F.);
#3092=ORIENTED_EDGE('',*,*,#2227,.F.);
#3093=ORIENTED_EDGE('',*,*,#2187,.F.);
#3094=ORIENTED_EDGE('',*,*,#2204,.F.);
#3095=ORIENTED_EDGE('',*,*,#2203,.F.);
#3096=ORIENTED_EDGE('',*,*,#2202,.F.);
#3097=ORIENTED_EDGE('',*,*,#2201,.F.);
#3098=ORIENTED_EDGE('',*,*,#2200,.F.);
#3099=ORIENTED_EDGE('',*,*,#2199,.F.);
#3100=ORIENTED_EDGE('',*,*,#2198,.F.);
#3101=ORIENTED_EDGE('',*,*,#2228,.F.);
#3102=ORIENTED_EDGE('',*,*,#2229,.T.);
#3103=ORIENTED_EDGE('',*,*,#2230,.T.);
#3104=ORIENTED_EDGE('',*,*,#2229,.F.);
#3105=ORIENTED_EDGE('',*,*,#2228,.T.);
#3106=ORIENTED_EDGE('',*,*,#2227,.T.);
#3107=ORIENTED_EDGE('',*,*,#2165,.T.);
#3108=ORIENTED_EDGE('',*,*,#2224,.F.);
#3109=ORIENTED_EDGE('',*,*,#2223,.T.);
#3110=ORIENTED_EDGE('',*,*,#2188,.F.);
#3111=ORIENTED_EDGE('',*,*,#2225,.T.);
#3112=ORIENTED_EDGE('',*,*,#2197,.T.);
#3113=ORIENTED_EDGE('',*,*,#2222,.T.);
#3114=ORIENTED_EDGE('',*,*,#2184,.T.);
#3115=ORIENTED_EDGE('',*,*,#2226,.T.);
#3116=ORIENTED_EDGE('',*,*,#2213,.T.);
#3117=ORIENTED_EDGE('',*,*,#2221,.T.);
#3118=ORIENTED_EDGE('',*,*,#2205,.T.);
#3119=ORIENTED_EDGE('',*,*,#2209,.T.);
#3120=ORIENTED_EDGE('',*,*,#2212,.T.);
#3121=ORIENTED_EDGE('',*,*,#2230,.F.);
#3122=ORIENTED_EDGE('',*,*,#2219,.T.);
#3123=ORIENTED_EDGE('',*,*,#2231,.T.);
#3124=ORIENTED_EDGE('',*,*,#2232,.T.);
#3125=ORIENTED_EDGE('',*,*,#2233,.T.);
#3126=ORIENTED_EDGE('',*,*,#2232,.F.);
#3127=ORIENTED_EDGE('',*,*,#2233,.F.);
#3128=ORIENTED_EDGE('',*,*,#2234,.F.);
#3129=ORIENTED_EDGE('',*,*,#2231,.F.);
#3130=ORIENTED_EDGE('',*,*,#2235,.T.);
#3131=ORIENTED_EDGE('',*,*,#2236,.T.);
#3132=ORIENTED_EDGE('',*,*,#2235,.F.);
#3133=ORIENTED_EDGE('',*,*,#2237,.F.);
#3134=ORIENTED_EDGE('',*,*,#2238,.F.);
#3135=ORIENTED_EDGE('',*,*,#2239,.T.);
#3136=ORIENTED_EDGE('',*,*,#2240,.F.);
#3137=ORIENTED_EDGE('',*,*,#2241,.F.);
#3138=ORIENTED_EDGE('',*,*,#2239,.F.);
#3139=ORIENTED_EDGE('',*,*,#2242,.F.);
#3140=ORIENTED_EDGE('',*,*,#2243,.T.);
#3141=ORIENTED_EDGE('',*,*,#2244,.T.);
#3142=ORIENTED_EDGE('',*,*,#2243,.F.);
#3143=ORIENTED_EDGE('',*,*,#2244,.F.);
#3144=ORIENTED_EDGE('',*,*,#2245,.T.);
#3145=ORIENTED_EDGE('',*,*,#2246,.F.);
#3146=ORIENTED_EDGE('',*,*,#2247,.T.);
#3147=ORIENTED_EDGE('',*,*,#2248,.T.);
#3148=ORIENTED_EDGE('',*,*,#2247,.F.);
#3149=ORIENTED_EDGE('',*,*,#2249,.F.);
#3150=ORIENTED_EDGE('',*,*,#2250,.T.);
#3151=ORIENTED_EDGE('',*,*,#2246,.T.);
#3152=ORIENTED_EDGE('',*,*,#2250,.F.);
#3153=ORIENTED_EDGE('',*,*,#2240,.T.);
#3154=ORIENTED_EDGE('',*,*,#2241,.T.);
#3155=ORIENTED_EDGE('',*,*,#2249,.T.);
#3156=ORIENTED_EDGE('',*,*,#2251,.T.);
#3157=ORIENTED_EDGE('',*,*,#2252,.F.);
#3158=ORIENTED_EDGE('',*,*,#2251,.F.);
#3159=ORIENTED_EDGE('',*,*,#2236,.F.);
#3160=ORIENTED_EDGE('',*,*,#2253,.T.);
#3161=ORIENTED_EDGE('',*,*,#2252,.T.);
#3162=ORIENTED_EDGE('',*,*,#2253,.F.);
#3163=ORIENTED_EDGE('',*,*,#2254,.F.);
#3164=ORIENTED_EDGE('',*,*,#2255,.T.);
#3165=ORIENTED_EDGE('',*,*,#2234,.T.);
#3166=ORIENTED_EDGE('',*,*,#2255,.F.);
#3167=ORIENTED_EDGE('',*,*,#2256,.F.);
#3168=ORIENTED_EDGE('',*,*,#2257,.T.);
#3169=ORIENTED_EDGE('',*,*,#2254,.T.);
#3170=ORIENTED_EDGE('',*,*,#2257,.F.);
#3171=ORIENTED_EDGE('',*,*,#2258,.F.);
#3172=ORIENTED_EDGE('',*,*,#2259,.T.);
#3173=ORIENTED_EDGE('',*,*,#2256,.T.);
#3174=ORIENTED_EDGE('',*,*,#2259,.F.);
#3175=ORIENTED_EDGE('',*,*,#2260,.F.);
#3176=ORIENTED_EDGE('',*,*,#2258,.T.);
#3177=ORIENTED_EDGE('',*,*,#2261,.F.);
#3178=ORIENTED_EDGE('',*,*,#2262,.T.);
#3179=ORIENTED_EDGE('',*,*,#2260,.T.);
#3180=ORIENTED_EDGE('',*,*,#2262,.F.);
#3181=ORIENTED_EDGE('',*,*,#2261,.T.);
#3182=ORIENTED_EDGE('',*,*,#2263,.F.);
#3183=ORIENTED_EDGE('',*,*,#2264,.F.);
#3184=ORIENTED_EDGE('',*,*,#2265,.T.);
#3185=ORIENTED_EDGE('',*,*,#2263,.T.);
#3186=ORIENTED_EDGE('',*,*,#2265,.F.);
#3187=ORIENTED_EDGE('',*,*,#2266,.F.);
#3188=ORIENTED_EDGE('',*,*,#2267,.T.);
#3189=ORIENTED_EDGE('',*,*,#2264,.T.);
#3190=ORIENTED_EDGE('',*,*,#2267,.F.);
#3191=ORIENTED_EDGE('',*,*,#2268,.F.);
#3192=ORIENTED_EDGE('',*,*,#2269,.T.);
#3193=ORIENTED_EDGE('',*,*,#2266,.T.);
#3194=ORIENTED_EDGE('',*,*,#2269,.F.);
#3195=ORIENTED_EDGE('',*,*,#2270,.F.);
#3196=ORIENTED_EDGE('',*,*,#2271,.T.);
#3197=ORIENTED_EDGE('',*,*,#2268,.T.);
#3198=ORIENTED_EDGE('',*,*,#2271,.F.);
#3199=ORIENTED_EDGE('',*,*,#2272,.F.);
#3200=ORIENTED_EDGE('',*,*,#2273,.T.);
#3201=ORIENTED_EDGE('',*,*,#2270,.T.);
#3202=ORIENTED_EDGE('',*,*,#2273,.F.);
#3203=ORIENTED_EDGE('',*,*,#2272,.T.);
#3204=ORIENTED_EDGE('',*,*,#2274,.F.);
#3205=ORIENTED_EDGE('',*,*,#2275,.F.);
#3206=ORIENTED_EDGE('',*,*,#2276,.T.);
#3207=ORIENTED_EDGE('',*,*,#2274,.T.);
#3208=ORIENTED_EDGE('',*,*,#2276,.F.);
#3209=ORIENTED_EDGE('',*,*,#2275,.T.);
#3210=ORIENTED_EDGE('',*,*,#2277,.F.);
#3211=ORIENTED_EDGE('',*,*,#2245,.F.);
#3212=ORIENTED_EDGE('',*,*,#2278,.T.);
#3213=ORIENTED_EDGE('',*,*,#2277,.T.);
#3214=ORIENTED_EDGE('',*,*,#2278,.F.);
#3215=ORIENTED_EDGE('',*,*,#2237,.T.);
#3216=ORIENTED_EDGE('',*,*,#2238,.T.);
#3217=ORIENTED_EDGE('',*,*,#2248,.F.);
#3218=ORIENTED_EDGE('',*,*,#2242,.T.);
#3219=ORIENTED_EDGE('',*,*,#2279,.T.);
#3220=ORIENTED_EDGE('',*,*,#2280,.T.);
#3221=ORIENTED_EDGE('',*,*,#2281,.T.);
#3222=ORIENTED_EDGE('',*,*,#2280,.F.);
#3223=ORIENTED_EDGE('',*,*,#2281,.F.);
#3224=ORIENTED_EDGE('',*,*,#2282,.T.);
#3225=ORIENTED_EDGE('',*,*,#2283,.F.);
#3226=ORIENTED_EDGE('',*,*,#2282,.F.);
#3227=ORIENTED_EDGE('',*,*,#2279,.F.);
#3228=ORIENTED_EDGE('',*,*,#2283,.T.);
#3229=ORIENTED_EDGE('',*,*,#2284,.T.);
#3230=ORIENTED_EDGE('',*,*,#2285,.T.);
#3231=ORIENTED_EDGE('',*,*,#2284,.F.);
#3232=ORIENTED_EDGE('',*,*,#2285,.F.);
#3233=ORIENTED_EDGE('',*,*,#2286,.F.);
#3234=ORIENTED_EDGE('',*,*,#2287,.T.);
#3235=ORIENTED_EDGE('',*,*,#2288,.T.);
#3236=ORIENTED_EDGE('',*,*,#2289,.T.);
#3237=ORIENTED_EDGE('',*,*,#2290,.T.);
#3238=ORIENTED_EDGE('',*,*,#2291,.T.);
#3239=ORIENTED_EDGE('',*,*,#2292,.T.);
#3240=ORIENTED_EDGE('',*,*,#2291,.F.);
#3241=ORIENTED_EDGE('',*,*,#2293,.T.);
#3242=ORIENTED_EDGE('',*,*,#2294,.T.);
#3243=ORIENTED_EDGE('',*,*,#2295,.T.);
#3244=ORIENTED_EDGE('',*,*,#2296,.T.);
#3245=ORIENTED_EDGE('',*,*,#2297,.F.);
#3246=ORIENTED_EDGE('',*,*,#2298,.T.);
#3247=ORIENTED_EDGE('',*,*,#2286,.T.);
#3248=ORIENTED_EDGE('',*,*,#2299,.T.);
#3249=ORIENTED_EDGE('',*,*,#2300,.F.);
#3250=ORIENTED_EDGE('',*,*,#2301,.T.);
#3251=ORIENTED_EDGE('',*,*,#2297,.T.);
#3252=ORIENTED_EDGE('',*,*,#2302,.T.);
#3253=ORIENTED_EDGE('',*,*,#2303,.F.);
#3254=ORIENTED_EDGE('',*,*,#2304,.T.);
#3255=ORIENTED_EDGE('',*,*,#2305,.T.);
#3256=ORIENTED_EDGE('',*,*,#2300,.T.);
#3257=ORIENTED_EDGE('',*,*,#2306,.T.);
#3258=ORIENTED_EDGE('',*,*,#2307,.T.);
#3259=ORIENTED_EDGE('',*,*,#2308,.F.);
#3260=ORIENTED_EDGE('',*,*,#2309,.T.);
#3261=ORIENTED_EDGE('',*,*,#2310,.T.);
#3262=ORIENTED_EDGE('',*,*,#2303,.T.);
#3263=ORIENTED_EDGE('',*,*,#2311,.T.);
#3264=ORIENTED_EDGE('',*,*,#2312,.T.);
#3265=ORIENTED_EDGE('',*,*,#2313,.F.);
#3266=ORIENTED_EDGE('',*,*,#2314,.T.);
#3267=ORIENTED_EDGE('',*,*,#2308,.T.);
#3268=ORIENTED_EDGE('',*,*,#2315,.T.);
#3269=ORIENTED_EDGE('',*,*,#2316,.F.);
#3270=ORIENTED_EDGE('',*,*,#2317,.T.);
#3271=ORIENTED_EDGE('',*,*,#2318,.T.);
#3272=ORIENTED_EDGE('',*,*,#2313,.T.);
#3273=ORIENTED_EDGE('',*,*,#2319,.T.);
#3274=ORIENTED_EDGE('',*,*,#2320,.T.);
#3275=ORIENTED_EDGE('',*,*,#2321,.F.);
#3276=ORIENTED_EDGE('',*,*,#2322,.T.);
#3277=ORIENTED_EDGE('',*,*,#2316,.T.);
#3278=ORIENTED_EDGE('',*,*,#2323,.T.);
#3279=ORIENTED_EDGE('',*,*,#2324,.F.);
#3280=ORIENTED_EDGE('',*,*,#2325,.T.);
#3281=ORIENTED_EDGE('',*,*,#2321,.T.);
#3282=ORIENTED_EDGE('',*,*,#2326,.T.);
#3283=ORIENTED_EDGE('',*,*,#2327,.F.);
#3284=ORIENTED_EDGE('',*,*,#2328,.T.);
#3285=ORIENTED_EDGE('',*,*,#2329,.T.);
#3286=ORIENTED_EDGE('',*,*,#2324,.T.);
#3287=ORIENTED_EDGE('',*,*,#2330,.T.);
#3288=ORIENTED_EDGE('',*,*,#2331,.T.);
#3289=ORIENTED_EDGE('',*,*,#2332,.F.);
#3290=ORIENTED_EDGE('',*,*,#2333,.T.);
#3291=ORIENTED_EDGE('',*,*,#2334,.T.);
#3292=ORIENTED_EDGE('',*,*,#2327,.T.);
#3293=ORIENTED_EDGE('',*,*,#2335,.T.);
#3294=ORIENTED_EDGE('',*,*,#2336,.T.);
#3295=ORIENTED_EDGE('',*,*,#2337,.F.);
#3296=ORIENTED_EDGE('',*,*,#2338,.T.);
#3297=ORIENTED_EDGE('',*,*,#2332,.T.);
#3298=ORIENTED_EDGE('',*,*,#2339,.T.);
#3299=ORIENTED_EDGE('',*,*,#2340,.F.);
#3300=ORIENTED_EDGE('',*,*,#2341,.T.);
#3301=ORIENTED_EDGE('',*,*,#2337,.T.);
#3302=ORIENTED_EDGE('',*,*,#2342,.T.);
#3303=ORIENTED_EDGE('',*,*,#2343,.F.);
#3304=ORIENTED_EDGE('',*,*,#2344,.F.);
#3305=ORIENTED_EDGE('',*,*,#2345,.F.);
#3306=ORIENTED_EDGE('',*,*,#2346,.T.);
#3307=ORIENTED_EDGE('',*,*,#2347,.F.);
#3308=ORIENTED_EDGE('',*,*,#2348,.F.);
#3309=ORIENTED_EDGE('',*,*,#2343,.T.);
#3310=ORIENTED_EDGE('',*,*,#2349,.T.);
#3311=ORIENTED_EDGE('',*,*,#2350,.F.);
#3312=ORIENTED_EDGE('',*,*,#2351,.F.);
#3313=ORIENTED_EDGE('',*,*,#2352,.F.);
#3314=ORIENTED_EDGE('',*,*,#2347,.T.);
#3315=ORIENTED_EDGE('',*,*,#2353,.T.);
#3316=ORIENTED_EDGE('',*,*,#2354,.F.);
#3317=ORIENTED_EDGE('',*,*,#2355,.F.);
#3318=ORIENTED_EDGE('',*,*,#2350,.T.);
#3319=ORIENTED_EDGE('',*,*,#2356,.T.);
#3320=ORIENTED_EDGE('',*,*,#2357,.F.);
#3321=ORIENTED_EDGE('',*,*,#2358,.F.);
#3322=ORIENTED_EDGE('',*,*,#2354,.T.);
#3323=ORIENTED_EDGE('',*,*,#2359,.T.);
#3324=ORIENTED_EDGE('',*,*,#2360,.F.);
#3325=ORIENTED_EDGE('',*,*,#2361,.F.);
#3326=ORIENTED_EDGE('',*,*,#2357,.T.);
#3327=ORIENTED_EDGE('',*,*,#2362,.T.);
#3328=ORIENTED_EDGE('',*,*,#2363,.F.);
#3329=ORIENTED_EDGE('',*,*,#2364,.F.);
#3330=ORIENTED_EDGE('',*,*,#2360,.T.);
#3331=ORIENTED_EDGE('',*,*,#2365,.T.);
#3332=ORIENTED_EDGE('',*,*,#2366,.F.);
#3333=ORIENTED_EDGE('',*,*,#2367,.F.);
#3334=ORIENTED_EDGE('',*,*,#2363,.T.);
#3335=ORIENTED_EDGE('',*,*,#2368,.T.);
#3336=ORIENTED_EDGE('',*,*,#2369,.F.);
#3337=ORIENTED_EDGE('',*,*,#2370,.F.);
#3338=ORIENTED_EDGE('',*,*,#2366,.T.);
#3339=ORIENTED_EDGE('',*,*,#2371,.T.);
#3340=ORIENTED_EDGE('',*,*,#2372,.F.);
#3341=ORIENTED_EDGE('',*,*,#2373,.F.);
#3342=ORIENTED_EDGE('',*,*,#2369,.T.);
#3343=ORIENTED_EDGE('',*,*,#2374,.T.);
#3344=ORIENTED_EDGE('',*,*,#2375,.F.);
#3345=ORIENTED_EDGE('',*,*,#2376,.F.);
#3346=ORIENTED_EDGE('',*,*,#2372,.T.);
#3347=ORIENTED_EDGE('',*,*,#2377,.T.);
#3348=ORIENTED_EDGE('',*,*,#2378,.F.);
#3349=ORIENTED_EDGE('',*,*,#2379,.F.);
#3350=ORIENTED_EDGE('',*,*,#2375,.T.);
#3351=ORIENTED_EDGE('',*,*,#2380,.T.);
#3352=ORIENTED_EDGE('',*,*,#2381,.T.);
#3353=ORIENTED_EDGE('',*,*,#2382,.F.);
#3354=ORIENTED_EDGE('',*,*,#2383,.F.);
#3355=ORIENTED_EDGE('',*,*,#2378,.T.);
#3356=ORIENTED_EDGE('',*,*,#2384,.T.);
#3357=ORIENTED_EDGE('',*,*,#2382,.T.);
#3358=ORIENTED_EDGE('',*,*,#2385,.T.);
#3359=ORIENTED_EDGE('',*,*,#2386,.F.);
#3360=ORIENTED_EDGE('',*,*,#2387,.F.);
#3361=ORIENTED_EDGE('',*,*,#2388,.F.);
#3362=ORIENTED_EDGE('',*,*,#2389,.F.);
#3363=ORIENTED_EDGE('',*,*,#2390,.T.);
#3364=ORIENTED_EDGE('',*,*,#2295,.F.);
#3365=ORIENTED_EDGE('',*,*,#2296,.F.);
#3366=ORIENTED_EDGE('',*,*,#2390,.F.);
#3367=ORIENTED_EDGE('',*,*,#2389,.T.);
#3368=ORIENTED_EDGE('',*,*,#2340,.T.);
#3369=ORIENTED_EDGE('',*,*,#2391,.T.);
#3370=ORIENTED_EDGE('',*,*,#2392,.F.);
#3371=ORIENTED_EDGE('',*,*,#2393,.T.);
#3372=ORIENTED_EDGE('',*,*,#2394,.F.);
#3373=ORIENTED_EDGE('',*,*,#2395,.F.);
#3374=ORIENTED_EDGE('',*,*,#2396,.T.);
#3375=ORIENTED_EDGE('',*,*,#2397,.T.);
#3376=ORIENTED_EDGE('',*,*,#2398,.T.);
#3377=ORIENTED_EDGE('',*,*,#2397,.F.);
#3378=ORIENTED_EDGE('',*,*,#2398,.F.);
#3379=ORIENTED_EDGE('',*,*,#2399,.T.);
#3380=ORIENTED_EDGE('',*,*,#2400,.F.);
#3381=ORIENTED_EDGE('',*,*,#2399,.F.);
#3382=ORIENTED_EDGE('',*,*,#2400,.T.);
#3383=ORIENTED_EDGE('',*,*,#2401,.T.);
#3384=ORIENTED_EDGE('',*,*,#2394,.T.);
#3385=ORIENTED_EDGE('',*,*,#2401,.F.);
#3386=ORIENTED_EDGE('',*,*,#2402,.F.);
#3387=ORIENTED_EDGE('',*,*,#2396,.F.);
#3388=ORIENTED_EDGE('',*,*,#2403,.F.);
#3389=ORIENTED_EDGE('',*,*,#2391,.F.);
#3390=ORIENTED_EDGE('',*,*,#2342,.F.);
#3391=ORIENTED_EDGE('',*,*,#2339,.F.);
#3392=ORIENTED_EDGE('',*,*,#2336,.F.);
#3393=ORIENTED_EDGE('',*,*,#2335,.F.);
#3394=ORIENTED_EDGE('',*,*,#2331,.F.);
#3395=ORIENTED_EDGE('',*,*,#2330,.F.);
#3396=ORIENTED_EDGE('',*,*,#2326,.F.);
#3397=ORIENTED_EDGE('',*,*,#2323,.F.);
#3398=ORIENTED_EDGE('',*,*,#2320,.F.);
#3399=ORIENTED_EDGE('',*,*,#2319,.F.);
#3400=ORIENTED_EDGE('',*,*,#2315,.F.);
#3401=ORIENTED_EDGE('',*,*,#2312,.F.);
#3402=ORIENTED_EDGE('',*,*,#2311,.F.);
#3403=ORIENTED_EDGE('',*,*,#2307,.F.);
#3404=ORIENTED_EDGE('',*,*,#2306,.F.);
#3405=ORIENTED_EDGE('',*,*,#2302,.F.);
#3406=ORIENTED_EDGE('',*,*,#2299,.F.);
#3407=ORIENTED_EDGE('',*,*,#2294,.F.);
#3408=ORIENTED_EDGE('',*,*,#2404,.F.);
#3409=ORIENTED_EDGE('',*,*,#2405,.T.);
#3410=ORIENTED_EDGE('',*,*,#2344,.T.);
#3411=ORIENTED_EDGE('',*,*,#2348,.T.);
#3412=ORIENTED_EDGE('',*,*,#2352,.T.);
#3413=ORIENTED_EDGE('',*,*,#2351,.T.);
#3414=ORIENTED_EDGE('',*,*,#2355,.T.);
#3415=ORIENTED_EDGE('',*,*,#2358,.T.);
#3416=ORIENTED_EDGE('',*,*,#2361,.T.);
#3417=ORIENTED_EDGE('',*,*,#2364,.T.);
#3418=ORIENTED_EDGE('',*,*,#2367,.T.);
#3419=ORIENTED_EDGE('',*,*,#2370,.T.);
#3420=ORIENTED_EDGE('',*,*,#2373,.T.);
#3421=ORIENTED_EDGE('',*,*,#2376,.T.);
#3422=ORIENTED_EDGE('',*,*,#2379,.T.);
#3423=ORIENTED_EDGE('',*,*,#2383,.T.);
#3424=ORIENTED_EDGE('',*,*,#2388,.T.);
#3425=ORIENTED_EDGE('',*,*,#2387,.T.);
#3426=ORIENTED_EDGE('',*,*,#2290,.F.);
#3427=ORIENTED_EDGE('',*,*,#2406,.T.);
#3428=ORIENTED_EDGE('',*,*,#2345,.T.);
#3429=ORIENTED_EDGE('',*,*,#2405,.F.);
#3430=ORIENTED_EDGE('',*,*,#2404,.T.);
#3431=ORIENTED_EDGE('',*,*,#2293,.F.);
#3432=ORIENTED_EDGE('',*,*,#2407,.F.);
#3433=ORIENTED_EDGE('',*,*,#2408,.F.);
#3434=ORIENTED_EDGE('',*,*,#2385,.F.);
#3435=ORIENTED_EDGE('',*,*,#2384,.F.);
#3436=ORIENTED_EDGE('',*,*,#2381,.F.);
#3437=ORIENTED_EDGE('',*,*,#2380,.F.);
#3438=ORIENTED_EDGE('',*,*,#2377,.F.);
#3439=ORIENTED_EDGE('',*,*,#2374,.F.);
#3440=ORIENTED_EDGE('',*,*,#2371,.F.);
#3441=ORIENTED_EDGE('',*,*,#2368,.F.);
#3442=ORIENTED_EDGE('',*,*,#2365,.F.);
#3443=ORIENTED_EDGE('',*,*,#2362,.F.);
#3444=ORIENTED_EDGE('',*,*,#2359,.F.);
#3445=ORIENTED_EDGE('',*,*,#2356,.F.);
#3446=ORIENTED_EDGE('',*,*,#2353,.F.);
#3447=ORIENTED_EDGE('',*,*,#2349,.F.);
#3448=ORIENTED_EDGE('',*,*,#2346,.F.);
#3449=ORIENTED_EDGE('',*,*,#2406,.F.);
#3450=ORIENTED_EDGE('',*,*,#2289,.F.);
#3451=ORIENTED_EDGE('',*,*,#2288,.F.);
#3452=ORIENTED_EDGE('',*,*,#2287,.F.);
#3453=ORIENTED_EDGE('',*,*,#2298,.F.);
#3454=ORIENTED_EDGE('',*,*,#2301,.F.);
#3455=ORIENTED_EDGE('',*,*,#2305,.F.);
#3456=ORIENTED_EDGE('',*,*,#2304,.F.);
#3457=ORIENTED_EDGE('',*,*,#2310,.F.);
#3458=ORIENTED_EDGE('',*,*,#2309,.F.);
#3459=ORIENTED_EDGE('',*,*,#2314,.F.);
#3460=ORIENTED_EDGE('',*,*,#2318,.F.);
#3461=ORIENTED_EDGE('',*,*,#2317,.F.);
#3462=ORIENTED_EDGE('',*,*,#2322,.F.);
#3463=ORIENTED_EDGE('',*,*,#2325,.F.);
#3464=ORIENTED_EDGE('',*,*,#2329,.F.);
#3465=ORIENTED_EDGE('',*,*,#2328,.F.);
#3466=ORIENTED_EDGE('',*,*,#2334,.F.);
#3467=ORIENTED_EDGE('',*,*,#2333,.F.);
#3468=ORIENTED_EDGE('',*,*,#2338,.F.);
#3469=ORIENTED_EDGE('',*,*,#2341,.F.);
#3470=ORIENTED_EDGE('',*,*,#2393,.F.);
#3471=ORIENTED_EDGE('',*,*,#2403,.T.);
#3472=ORIENTED_EDGE('',*,*,#2386,.T.);
#3473=ORIENTED_EDGE('',*,*,#2408,.T.);
#3474=ORIENTED_EDGE('',*,*,#2407,.T.);
#3475=ORIENTED_EDGE('',*,*,#2392,.T.);
#3476=ORIENTED_EDGE('',*,*,#2409,.T.);
#3477=ORIENTED_EDGE('',*,*,#2410,.T.);
#3478=ORIENTED_EDGE('',*,*,#2411,.T.);
#3479=ORIENTED_EDGE('',*,*,#2410,.F.);
#3480=ORIENTED_EDGE('',*,*,#2411,.F.);
#3481=ORIENTED_EDGE('',*,*,#2412,.T.);
#3482=ORIENTED_EDGE('',*,*,#2413,.T.);
#3483=ORIENTED_EDGE('',*,*,#2412,.F.);
#3484=ORIENTED_EDGE('',*,*,#2409,.F.);
#3485=ORIENTED_EDGE('',*,*,#2292,.F.);
#3486=ORIENTED_EDGE('',*,*,#2414,.T.);
#3487=ORIENTED_EDGE('',*,*,#2415,.T.);
#3488=ORIENTED_EDGE('',*,*,#2416,.T.);
#3489=ORIENTED_EDGE('',*,*,#2415,.F.);
#3490=ORIENTED_EDGE('',*,*,#2416,.F.);
#3491=ORIENTED_EDGE('',*,*,#2417,.T.);
#3492=ORIENTED_EDGE('',*,*,#2418,.F.);
#3493=ORIENTED_EDGE('',*,*,#2417,.F.);
#3494=ORIENTED_EDGE('',*,*,#2414,.F.);
#3495=ORIENTED_EDGE('',*,*,#2413,.F.);
#3496=ORIENTED_EDGE('',*,*,#2418,.T.);
#3497=ORIENTED_EDGE('',*,*,#2419,.T.);
#3498=ORIENTED_EDGE('',*,*,#2420,.T.);
#3499=ORIENTED_EDGE('',*,*,#2419,.F.);
#3500=ORIENTED_EDGE('',*,*,#2420,.F.);
#3501=ORIENTED_EDGE('',*,*,#2421,.T.);
#3502=ORIENTED_EDGE('',*,*,#2422,.T.);
#3503=ORIENTED_EDGE('',*,*,#2423,.T.);
#3504=ORIENTED_EDGE('',*,*,#2424,.T.);
#3505=ORIENTED_EDGE('',*,*,#2423,.F.);
#3506=ORIENTED_EDGE('',*,*,#2424,.F.);
#3507=ORIENTED_EDGE('',*,*,#2425,.T.);
#3508=ORIENTED_EDGE('',*,*,#2426,.F.);
#3509=ORIENTED_EDGE('',*,*,#2425,.F.);
#3510=ORIENTED_EDGE('',*,*,#2422,.F.);
#3511=ORIENTED_EDGE('',*,*,#2427,.F.);
#3512=ORIENTED_EDGE('',*,*,#2426,.T.);
#3513=ORIENTED_EDGE('',*,*,#2428,.T.);
#3514=ORIENTED_EDGE('',*,*,#2402,.T.);
#3515=ORIENTED_EDGE('',*,*,#2428,.F.);
#3516=ORIENTED_EDGE('',*,*,#2395,.T.);
#3517=ORIENTED_EDGE('',*,*,#2429,.T.);
#3518=ORIENTED_EDGE('',*,*,#2430,.T.);
#3519=ORIENTED_EDGE('',*,*,#2429,.F.);
#3520=ORIENTED_EDGE('',*,*,#2430,.F.);
#3521=ORIENTED_EDGE('',*,*,#2431,.T.);
#3522=ORIENTED_EDGE('',*,*,#2432,.F.);
#3523=ORIENTED_EDGE('',*,*,#2431,.F.);
#3524=ORIENTED_EDGE('',*,*,#2432,.T.);
#3525=ORIENTED_EDGE('',*,*,#2433,.T.);
#3526=ORIENTED_EDGE('',*,*,#2434,.T.);
#3527=ORIENTED_EDGE('',*,*,#2433,.F.);
#3528=ORIENTED_EDGE('',*,*,#2434,.F.);
#3529=ORIENTED_EDGE('',*,*,#2435,.T.);
#3530=ORIENTED_EDGE('',*,*,#2436,.T.);
#3531=ORIENTED_EDGE('',*,*,#2437,.T.);
#3532=ORIENTED_EDGE('',*,*,#2438,.T.);
#3533=ORIENTED_EDGE('',*,*,#2437,.F.);
#3534=ORIENTED_EDGE('',*,*,#2438,.F.);
#3535=ORIENTED_EDGE('',*,*,#2439,.T.);
#3536=ORIENTED_EDGE('',*,*,#2440,.F.);
#3537=ORIENTED_EDGE('',*,*,#2439,.F.);
#3538=ORIENTED_EDGE('',*,*,#2436,.F.);
#3539=ORIENTED_EDGE('',*,*,#2441,.F.);
#3540=ORIENTED_EDGE('',*,*,#2440,.T.);
#3541=ORIENTED_EDGE('',*,*,#2442,.T.);
#3542=ORIENTED_EDGE('',*,*,#2443,.T.);
#3543=ORIENTED_EDGE('',*,*,#2442,.F.);
#3544=ORIENTED_EDGE('',*,*,#2443,.F.);
#3545=ORIENTED_EDGE('',*,*,#2444,.T.);
#3546=ORIENTED_EDGE('',*,*,#2445,.T.);
#3547=ORIENTED_EDGE('',*,*,#2446,.T.);
#3548=ORIENTED_EDGE('',*,*,#2447,.T.);
#3549=ORIENTED_EDGE('',*,*,#2446,.F.);
#3550=ORIENTED_EDGE('',*,*,#2447,.F.);
#3551=ORIENTED_EDGE('',*,*,#2444,.F.);
#3552=ORIENTED_EDGE('',*,*,#2448,.T.);
#3553=ORIENTED_EDGE('',*,*,#2445,.F.);
#3554=ORIENTED_EDGE('',*,*,#2448,.F.);
#3555=ORIENTED_EDGE('',*,*,#2435,.F.);
#3556=ORIENTED_EDGE('',*,*,#2449,.T.);
#3557=ORIENTED_EDGE('',*,*,#2441,.T.);
#3558=ORIENTED_EDGE('',*,*,#2449,.F.);
#3559=ORIENTED_EDGE('',*,*,#2421,.F.);
#3560=ORIENTED_EDGE('',*,*,#2450,.T.);
#3561=ORIENTED_EDGE('',*,*,#2427,.T.);
#3562=ORIENTED_EDGE('',*,*,#2450,.F.);
#3563=ORIENTED_EDGE('',*,*,#2451,.F.);
#3564=ORIENTED_EDGE('',*,*,#2452,.T.);
#3565=ORIENTED_EDGE('',*,*,#2453,.T.);
#3566=ORIENTED_EDGE('',*,*,#2452,.F.);
#3567=ORIENTED_EDGE('',*,*,#2451,.T.);
#3568=ORIENTED_EDGE('',*,*,#2454,.F.);
#3569=ORIENTED_EDGE('',*,*,#2455,.F.);
#3570=ORIENTED_EDGE('',*,*,#2456,.T.);
#3571=ORIENTED_EDGE('',*,*,#2454,.T.);
#3572=ORIENTED_EDGE('',*,*,#2456,.F.);
#3573=ORIENTED_EDGE('',*,*,#2453,.F.);
#3574=ORIENTED_EDGE('',*,*,#2455,.T.);
#3575=B_SPLINE_SURFACE_WITH_KNOTS('',3,1,((#5132,#5133),(#5134,#5135),(#5136,
#5137),(#5138,#5139),(#5140,#5141),(#5142,#5143),(#5144,#5145),(#5146,#5147),
(#5148,#5149),(#5150,#5151),(#5152,#5153),(#5154,#5155),(#5156,#5157),(#5158,
#5159)),.UNSPECIFIED.,.F.,.F.,.F.,(4,2,2,2,2,2,4),(2,2),(-0.844212290556731,
-0.730966332817565,-0.619975754240938,-0.457326579004558,-0.29977928179387,
-0.147336283383114,0.),(0.,0.575999999999998),.UNSPECIFIED.);
#3576=B_SPLINE_SURFACE_WITH_KNOTS('',3,1,((#5200,#5201),(#5202,#5203),(#5204,
#5205),(#5206,#5207),(#5208,#5209),(#5210,#5211),(#5212,#5213),(#5214,#5215),
(#5216,#5217),(#5218,#5219),(#5220,#5221),(#5222,#5223),(#5224,#5225),(#5226,
#5227)),.UNSPECIFIED.,.F.,.F.,.F.,(4,2,2,2,2,2,4),(2,2),(-0.847325527525843,
-0.749719327139836,-0.649860858750851,-0.495073659399383,-0.335166304629316,
-0.170141007879843,0.),(0.,0.575999999999998),.UNSPECIFIED.);
#3577=B_SPLINE_SURFACE_WITH_KNOTS('',3,1,((#5416,#5417),(#5418,#5419),(#5420,
#5421),(#5422,#5423),(#5424,#5425),(#5426,#5427),(#5428,#5429),(#5430,#5431),
(#5432,#5433),(#5434,#5435),(#5436,#5437),(#5438,#5439),(#5440,#5441),(#5442,
#5443)),.UNSPECIFIED.,.F.,.F.,.F.,(4,2,2,2,2,2,4),(2,2),(-0.844212290556731,
-0.730966332817565,-0.619975754240938,-0.457326579004558,-0.29977928179387,
-0.147336283383114,0.),(0.,0.576),.UNSPECIFIED.);
#3578=B_SPLINE_SURFACE_WITH_KNOTS('',3,1,((#5484,#5485),(#5486,#5487),(#5488,
#5489),(#5490,#5491),(#5492,#5493),(#5494,#5495),(#5496,#5497),(#5498,#5499),
(#5500,#5501),(#5502,#5503),(#5504,#5505),(#5506,#5507),(#5508,#5509),(#5510,
#5511)),.UNSPECIFIED.,.F.,.F.,.F.,(4,2,2,2,2,2,4),(2,2),(-0.847325527525843,
-0.749719327139836,-0.649860858750851,-0.495073659399383,-0.335166304629316,
-0.170141007879843,0.),(0.,0.576),.UNSPECIFIED.);
#3579=B_SPLINE_SURFACE_WITH_KNOTS('',3,3,((#6564,#6565,#6566,#6567),(#6568,
#6569,#6570,#6571),(#6572,#6573,#6574,#6575),(#6576,#6577,#6578,#6579)),
 .UNSPECIFIED.,.F.,.F.,.F.,(4,4),(4,4),(0.066620174713851,0.0820126057383863),
(8.314732749858,8.70158673567856),.UNSPECIFIED.);
#3580=B_SPLINE_SURFACE_WITH_KNOTS('',3,3,((#6586,#6587,#6588,#6589,#6590,
#6591),(#6592,#6593,#6594,#6595,#6596,#6597),(#6598,#6599,#6600,#6601,#6602,
#6603),(#6604,#6605,#6606,#6607,#6608,#6609)),.UNSPECIFIED.,.F.,.F.,.F.,
(4,4),(4,1,1,4),(-0.000200320262106561,0.0820126057383863),(47.6103505270742,
48.3332993342991,49.0560729269844,49.7790217342094),.UNSPECIFIED.);
#3581=B_SPLINE_SURFACE_WITH_KNOTS('',3,3,((#6665,#6666,#6667,#6668,#6669,
#6670),(#6671,#6672,#6673,#6674,#6675,#6676),(#6677,#6678,#6679,#6680,#6681,
#6682),(#6683,#6684,#6685,#6686,#6687,#6688)),.UNSPECIFIED.,.F.,.F.,.F.,
(4,4),(4,1,1,4),(-0.000197985600878005,0.0820126057383863),(41.3271643941354,
42.0501140271196,42.7728876198048,43.495837252789),.UNSPECIFIED.);
#3582=B_SPLINE_SURFACE_WITH_KNOTS('',3,3,((#6695,#6696,#6697,#6698,#6699,
#6700),(#6701,#6702,#6703,#6704,#6705,#6706),(#6707,#6708,#6709,#6710,#6711,
#6712),(#6713,#6714,#6715,#6716,#6717,#6718)),.UNSPECIFIED.,.F.,.F.,.F.,
(4,4),(4,1,1,4),(-0.000195813814893523,0.0820126057383863),(35.0439783465439,
35.76692871994,36.4897023126252,37.2126526860213),.UNSPECIFIED.);
#3583=B_SPLINE_SURFACE_WITH_KNOTS('',3,3,((#6725,#6726,#6727,#6728,#6729,
#6730),(#6731,#6732,#6733,#6734,#6735,#6736),(#6737,#6738,#6739,#6740,#6741,
#6742),(#6743,#6744,#6745,#6746,#6747,#6748)),.UNSPECIFIED.,.F.,.F.,.F.,
(4,4),(4,1,1,4),(-0.000193785406214375,0.0820126057383863),(28.7607923707967,
29.4837434127604,30.2065170054456,30.9294680474093),.UNSPECIFIED.);
#3584=B_SPLINE_SURFACE_WITH_KNOTS('',3,3,((#6755,#6756,#6757,#6758,#6759,
#6760),(#6761,#6762,#6763,#6764,#6765,#6766),(#6767,#6768,#6769,#6770,#6771,
#6772),(#6773,#6774,#6775,#6776,#6777,#6778)),.UNSPECIFIED.,.F.,.F.,.F.,
(4,4),(4,1,1,4),(-0.000191884308595516,0.0820126057383863),(22.4776064561872,
23.2005581055808,23.9233316982661,24.6462833476596),.UNSPECIFIED.);
#3585=B_SPLINE_SURFACE_WITH_KNOTS('',3,3,((#6785,#6786,#6787,#6788,#6789,
#6790),(#6791,#6792,#6793,#6794,#6795,#6796),(#6797,#6798,#6799,#6800,#6801,
#6802),(#6803,#6804,#6805,#6806,#6807,#6808)),.UNSPECIFIED.,.F.,.F.,.F.,
(4,4),(4,1,1,4),(-0.000190097099794286,0.0820126057383863),(16.1944205941067,
16.9173727984012,17.6401463910865,18.363098595381),.UNSPECIFIED.);
#3586=B_SPLINE_SURFACE_WITH_KNOTS('',3,3,((#6815,#6816,#6817,#6818,#6819,
#6820),(#6821,#6822,#6823,#6824,#6825,#6826),(#6827,#6828,#6829,#6830,#6831,
#6832),(#6833,#6834,#6835,#6836,#6837,#6838)),.UNSPECIFIED.,.F.,.F.,.F.,
(4,4),(4,1,1,4),(-0.000156396744294902,0.0821188966323171),(9.98287940740301,
10.6818311637994,11.3807829201958,12.0798910733364),.UNSPECIFIED.);
#3587=B_SPLINE_SURFACE_WITH_KNOTS('',3,3,((#6907,#6908,#6909,#6910,#6911,
#6912),(#6913,#6914,#6915,#6916,#6917,#6918),(#6919,#6920,#6921,#6922,#6923,
#6924),(#6925,#6926,#6927,#6928,#6929,#6930)),.UNSPECIFIED.,.F.,.F.,.F.,
(4,4),(4,1,1,4),(-0.000199131191863258,0.0820126057383863),(44.4687574489585,
45.1917066807094,45.9144802733946,46.6374295051455),.UNSPECIFIED.);
#3588=B_SPLINE_SURFACE_WITH_KNOTS('',3,3,((#6937,#6938,#6939,#6940,#6941,
#6942),(#6943,#6944,#6945,#6946,#6947,#6948),(#6949,#6950,#6951,#6952,#6953,
#6954),(#6955,#6956,#6957,#6958,#6959,#6960)),.UNSPECIFIED.,.F.,.F.,.F.,
(4,4),(4,1,1,4),(-0.000196880658646492,0.0820126057383863),(38.1855713605906,
38.9085213735298,39.631294966215,40.3542449791542),.UNSPECIFIED.);
#3589=B_SPLINE_SURFACE_WITH_KNOTS('',3,3,((#6967,#6968,#6969,#6970,#6971,
#6972),(#6973,#6974,#6975,#6976,#6977,#6978),(#6979,#6980,#6981,#6982,#6983,
#6984),(#6985,#6986,#6987,#6988,#6989,#6990)),.UNSPECIFIED.,.F.,.F.,.F.,
(4,4),(4,1,1,4),(-0.000194782762460684,0.0820126057383863),(31.9023853504151,
32.6253360663502,33.3481096590354,34.0710603749705),.UNSPECIFIED.);
#3590=B_SPLINE_SURFACE_WITH_KNOTS('',3,3,((#6997,#6998,#6999,#7000,#7001,
#7002),(#7003,#7004,#7005,#7006,#7007,#7008),(#7009,#7010,#7011,#7012,#7013,
#7014),(#7015,#7016,#7017,#7018,#7019,#7020)),.UNSPECIFIED.,.F.,.F.,.F.,
(4,4),(4,1,1,4),(-0.000192819836832936,0.0820126057383863),(25.6191994064303,
26.3421507591706,27.0649243518558,27.7878757045961),.UNSPECIFIED.);
#3591=B_SPLINE_SURFACE_WITH_KNOTS('',3,3,((#7027,#7028,#7029,#7030,#7031,
#7032),(#7033,#7034,#7035,#7036,#7037,#7038),(#7039,#7040,#7041,#7042,#7043,
#7044),(#7045,#7046,#7047,#7048,#7049,#7050)),.UNSPECIFIED.,.F.,.F.,.F.,
(4,4),(4,1,1,4),(-0.000190977220451414,0.0820126057383863),(19.3360135190516,
20.058965451991,20.7817390446763,21.5046909776157),.UNSPECIFIED.);
#3592=B_SPLINE_SURFACE_WITH_KNOTS('',3,3,((#7057,#7058,#7059,#7060,#7061,
#7062),(#7063,#7064,#7065,#7066,#7067,#7068),(#7069,#7070,#7071,#7072,#7073,
#7074),(#7075,#7076,#7077,#7078,#7079,#7080)),.UNSPECIFIED.,.F.,.F.,.F.,
(4,4),(4,1,1,4),(-0.000189242588512825,0.0820126057383863),(13.0528276805227,
13.7757801448114,14.4985537374967,15.2215062017854),.UNSPECIFIED.);
#3593=B_SPLINE_SURFACE_WITH_KNOTS('',3,3,((#7281,#7282,#7283,#7284,#7285,
#7286),(#7287,#7288,#7289,#7290,#7291,#7292),(#7293,#7294,#7295,#7296,#7297,
#7298),(#7299,#7300,#7301,#7302,#7303,#7304)),.UNSPECIFIED.,.F.,.F.,.F.,
(4,4),(4,1,1,4),(0.,0.0822109230065992),(47.6103498167155,48.3332993342991,
49.0560729269844,49.7790224445681),.UNSPECIFIED.);
#3594=B_SPLINE_SURFACE_WITH_KNOTS('',3,3,((#7305,#7306,#7307,#7308,#7309,
#7310),(#7311,#7312,#7313,#7314,#7315,#7316),(#7317,#7318,#7319,#7320,#7321,
#7322),(#7323,#7324,#7325,#7326,#7327,#7328)),.UNSPECIFIED.,.F.,.F.,.F.,
(4,4),(4,1,1,4),(0.,0.0822087286475259),(41.3271637575297,42.0501140271195,
42.7728876198048,43.4958378893947),.UNSPECIFIED.);
#3595=B_SPLINE_SURFACE_WITH_KNOTS('',3,3,((#7329,#7330,#7331,#7332,#7333,
#7334),(#7335,#7336,#7337,#7338,#7339,#7340),(#7341,#7342,#7343,#7344,#7345,
#7346),(#7347,#7348,#7349,#7350,#7351,#7352)),.UNSPECIFIED.,.F.,.F.,.F.,
(4,4),(4,1,1,4),(0.,0.0822066802882628),(35.0439777719737,35.76692871994,
36.4897023126252,37.2126532605915),.UNSPECIFIED.);
#3596=B_SPLINE_SURFACE_WITH_KNOTS('',3,3,((#7353,#7354,#7355,#7356,#7357,
#7358),(#7359,#7360,#7361,#7362,#7363,#7364),(#7365,#7366,#7367,#7368,#7369,
#7370),(#7371,#7372,#7373,#7374,#7375,#7376)),.UNSPECIFIED.,.F.,.F.,.F.,
(4,4),(4,1,1,4),(0.,0.0822047614148872),(28.7607918489802,29.4837434127604,
30.2065170054456,30.9294685692258),.UNSPECIFIED.);
#3597=B_SPLINE_SURFACE_WITH_KNOTS('',3,3,((#7377,#7378,#7379,#7380,#7381,
#7382),(#7383,#7384,#7385,#7386,#7387,#7388),(#7389,#7390,#7391,#7392,#7393,
#7394),(#7395,#7396,#7397,#7398,#7399,#7400)),.UNSPECIFIED.,.F.,.F.,.F.,
(4,4),(4,1,1,4),(0.,0.0822029582573803),(22.4776059796679,23.2005581055808,
23.9233316982661,24.6462838241789),.UNSPECIFIED.);
#3598=B_SPLINE_SURFACE_WITH_KNOTS('',3,3,((#7401,#7402,#7403,#7404,#7405,
#7406),(#7407,#7408,#7409,#7410,#7411,#7412),(#7413,#7414,#7415,#7416,#7417,
#7418),(#7419,#7420,#7421,#7422,#7423,#7424)),.UNSPECIFIED.,.F.,.F.,.F.,
(4,4),(4,1,1,4),(0.,0.082201259192146),(16.1944201568192,16.9173727984012,
17.6401463910865,18.3630990326685),.UNSPECIFIED.);
#3599=B_SPLINE_SURFACE_WITH_KNOTS('',3,3,((#7425,#7426,#7427,#7428,#7429,
#7430),(#7431,#7432,#7433,#7434,#7435,#7436),(#7437,#7438,#7439,#7440,#7441,
#7442),(#7443,#7444,#7445,#7446,#7447,#7448)),.UNSPECIFIED.,.F.,.F.,.F.,
(4,4),(4,1,1,4),(-9.65518509377315E-5,0.0821438972802576),(50.7519871036618,
51.4243296588263,52.0965409224489,52.7687521860715),.UNSPECIFIED.);
#3600=B_SPLINE_SURFACE_WITH_KNOTS('',3,3,((#7449,#7450,#7451,#7452,#7453,
#7454),(#7455,#7456,#7457,#7458,#7459,#7460),(#7461,#7462,#7463,#7464,#7465,
#7466),(#7467,#7468,#7469,#7470,#7471,#7472)),.UNSPECIFIED.,.F.,.F.,.F.,
(4,4),(4,1,1,4),(0.,0.08220980641716),(44.4687567771236,45.1917066807094,
45.9144802733946,46.6374301769804),.UNSPECIFIED.);
#3601=B_SPLINE_SURFACE_WITH_KNOTS('',3,3,((#7473,#7474,#7475,#7476,#7477,
#7478),(#7479,#7480,#7481,#7482,#7483,#7484),(#7485,#7486,#7487,#7488,#7489,
#7490),(#7491,#7492,#7493,#7494,#7495,#7496)),.UNSPECIFIED.,.F.,.F.,.F.,
(4,4),(4,1,1,4),(0.,0.0822076873226976),(38.1855707562983,38.9085213735298,
39.631294966215,40.3542455834465),.UNSPECIFIED.);
#3602=B_SPLINE_SURFACE_WITH_KNOTS('',3,3,((#7497,#7498,#7499,#7500,#7501,
#7502),(#7503,#7504,#7505,#7506,#7507,#7508),(#7509,#7510,#7511,#7512,#7513,
#7514),(#7515,#7516,#7517,#7518,#7519,#7520)),.UNSPECIFIED.,.F.,.F.,.F.,
(4,4),(4,1,1,4),(0.,0.0822057055828623),(31.902384803256,32.6253360663502,
33.3481096590354,34.0710609221296),.UNSPECIFIED.);
#3603=B_SPLINE_SURFACE_WITH_KNOTS('',3,3,((#7521,#7522,#7523,#7524,#7525,
#7526),(#7527,#7528,#7529,#7530,#7531,#7532),(#7533,#7534,#7535,#7536,#7537,
#7538),(#7539,#7540,#7541,#7542,#7543,#7544)),.UNSPECIFIED.,.F.,.F.,.F.,
(4,4),(4,1,1,4),(0.,0.0822038461426398),(25.619198908099,26.3421507591706,
27.0649243518559,27.7878762029274),.UNSPECIFIED.);
#3604=B_SPLINE_SURFACE_WITH_KNOTS('',3,3,((#7545,#7546,#7547,#7548,#7549,
#7550),(#7551,#7552,#7553,#7554,#7555,#7556),(#7557,#7558,#7559,#7560,#7561,
#7562),(#7563,#7564,#7565,#7566,#7567,#7568)),.UNSPECIFIED.,.F.,.F.,.F.,
(4,4),(4,1,1,4),(0.,0.0822020963687411),(19.3360130628329,20.058965451991,
20.7817390446763,21.5046914338344),.UNSPECIFIED.);
#3605=B_SPLINE_SURFACE_WITH_KNOTS('',3,3,((#7569,#7570,#7571,#7572,#7573,
#7574),(#7575,#7576,#7577,#7578,#7579,#7580),(#7581,#7582,#7583,#7584,#7585,
#7586),(#7587,#7588,#7589,#7590,#7591,#7592)),.UNSPECIFIED.,.F.,.F.,.F.,
(4,4),(4,1,1,4),(0.,0.0822004455378898),(13.0528272609226,13.7757801448114,
14.4985537374967,15.2215066213855),.UNSPECIFIED.);
#3606=B_SPLINE_SURFACE_WITH_KNOTS('',3,3,((#7594,#7595,#7596,#7597),(#7598,
#7599,#7600,#7601),(#7602,#7603,#7604,#7605),(#7606,#7607,#7608,#7609)),
 .UNSPECIFIED.,.F.,.F.,.F.,(4,4),(4,4),(0.0663734465876268,0.0820126057383863),
(11.6152142277547,12.0797346765921),.UNSPECIFIED.);
#3607=B_SPLINE_SURFACE_WITH_KNOTS('',3,3,((#14281,#14282,#14283,#14284,
#14285,#14286),(#14287,#14288,#14289,#14290,#14291,#14292),(#14293,#14294,
#14295,#14296,#14297,#14298),(#14299,#14300,#14301,#14302,#14303,#14304)),
 .UNSPECIFIED.,.F.,.F.,.F.,(4,4),(4,1,1,4),(0.,0.0494711118308268),(16.7019134878289,
17.6517088926312,18.6014255011318,19.5511421096324),.UNSPECIFIED.);
#3608=B_SPLINE_SURFACE_WITH_KNOTS('',3,3,((#14515,#14516,#14517,#14518,
#14519,#14520),(#14521,#14522,#14523,#14524,#14525,#14526),(#14527,#14528,
#14529,#14530,#14531,#14532),(#14533,#14534,#14535,#14536,#14537,#14538)),
 .UNSPECIFIED.,.F.,.F.,.F.,(4,4),(4,1,1,4),(-7.87913040489834E-5,0.0493923155291723),
(13.3942556087771,14.3439722172777,15.2936888257783,16.2434842255829),
 .UNSPECIFIED.);
#3609=B_SPLINE_SURFACE_WITH_KNOTS('',3,3,((#14729,#14730,#14731,#14732,
#14733,#14734,#14735,#14736,#14737,#14738,#14739,#14740,#14741,#14742,#14743,
#14744,#14745,#14746,#14747,#14748,#14749,#14750,#14751,#14752,#14753,#14754,
#14755,#14756,#14757,#14758,#14759,#14760,#14761,#14762,#14763,#14764,#14765,
#14766,#14767,#14768,#14769,#14770,#14771,#14772,#14773,#14774,#14775,#14776),
(#14777,#14778,#14779,#14780,#14781,#14782,#14783,#14784,#14785,#14786,
#14787,#14788,#14789,#14790,#14791,#14792,#14793,#14794,#14795,#14796,#14797,
#14798,#14799,#14800,#14801,#14802,#14803,#14804,#14805,#14806,#14807,#14808,
#14809,#14810,#14811,#14812,#14813,#14814,#14815,#14816,#14817,#14818,#14819,
#14820,#14821,#14822,#14823,#14824),(#14825,#14826,#14827,#14828,#14829,
#14830,#14831,#14832,#14833,#14834,#14835,#14836,#14837,#14838,#14839,#14840,
#14841,#14842,#14843,#14844,#14845,#14846,#14847,#14848,#14849,#14850,#14851,
#14852,#14853,#14854,#14855,#14856,#14857,#14858,#14859,#14860,#14861,#14862,
#14863,#14864,#14865,#14866,#14867,#14868,#14869,#14870,#14871,#14872),
(#14873,#14874,#14875,#14876,#14877,#14878,#14879,#14880,#14881,#14882,
#14883,#14884,#14885,#14886,#14887,#14888,#14889,#14890,#14891,#14892,#14893,
#14894,#14895,#14896,#14897,#14898,#14899,#14900,#14901,#14902,#14903,#14904,
#14905,#14906,#14907,#14908,#14909,#14910,#14911,#14912,#14913,#14914,#14915,
#14916,#14917,#14918,#14919,#14920)),.UNSPECIFIED.,.F.,.F.,.F.,(4,4),(4,
1,1,1,1,1,1,1,1,1,1,1,1,1,1,1,1,1,1,1,1,1,1,1,1,1,1,1,1,1,1,1,1,1,1,1,1,
1,1,1,1,1,1,1,1,4),(-0.000683464176930082,0.0827553131308724),(8.31487785380719,
8.80643119756841,9.29798454132964,10.2810912288521,11.2641979163745,12.247304603897,
13.2304112914194,14.2135179789419,15.1966246664643,16.1797313539867,17.1628380415092,
18.1459447290316,19.1290514165541,20.1121581040765,21.095264791599,22.0783714791214,
23.0614781666439,24.0445848541663,25.0276915416888,26.0107982292112,26.9939049167336,
27.9770116042561,28.9601182917785,29.943224979301,30.9263316668234,31.9094383543459,
32.8925450418683,33.8756517293908,34.8587584169132,35.8418651044356,36.8249717919581,
37.8080784794805,38.791185167003,39.7742918545254,40.7573985420479,41.7405052295703,
42.7236119170928,43.7067186046152,44.6898252921376,45.6729319796601,46.6560386671825,
47.639145354705,48.6222520422274,49.6053587297499,50.0969120735111,50.5891488814492),
 .UNSPECIFIED.);
#3610=B_SPLINE_SURFACE_WITH_KNOTS('',3,3,((#15129,#15130,#15131,#15132,
#15133,#15134,#15135,#15136,#15137,#15138,#15139,#15140,#15141,#15142,#15143,
#15144,#15145,#15146,#15147,#15148,#15149,#15150,#15151,#15152,#15153,#15154,
#15155,#15156,#15157,#15158,#15159,#15160,#15161,#15162,#15163,#15164,#15165,
#15166,#15167,#15168,#15169,#15170,#15171,#15172,#15173,#15174,#15175,#15176),
(#15177,#15178,#15179,#15180,#15181,#15182,#15183,#15184,#15185,#15186,
#15187,#15188,#15189,#15190,#15191,#15192,#15193,#15194,#15195,#15196,#15197,
#15198,#15199,#15200,#15201,#15202,#15203,#15204,#15205,#15206,#15207,#15208,
#15209,#15210,#15211,#15212,#15213,#15214,#15215,#15216,#15217,#15218,#15219,
#15220,#15221,#15222,#15223,#15224),(#15225,#15226,#15227,#15228,#15229,
#15230,#15231,#15232,#15233,#15234,#15235,#15236,#15237,#15238,#15239,#15240,
#15241,#15242,#15243,#15244,#15245,#15246,#15247,#15248,#15249,#15250,#15251,
#15252,#15253,#15254,#15255,#15256,#15257,#15258,#15259,#15260,#15261,#15262,
#15263,#15264,#15265,#15266,#15267,#15268,#15269,#15270,#15271,#15272),
(#15273,#15274,#15275,#15276,#15277,#15278,#15279,#15280,#15281,#15282,
#15283,#15284,#15285,#15286,#15287,#15288,#15289,#15290,#15291,#15292,#15293,
#15294,#15295,#15296,#15297,#15298,#15299,#15300,#15301,#15302,#15303,#15304,
#15305,#15306,#15307,#15308,#15309,#15310,#15311,#15312,#15313,#15314,#15315,
#15316,#15317,#15318,#15319,#15320)),.UNSPECIFIED.,.F.,.F.,.F.,(4,4),(4,
1,1,1,1,1,1,1,1,1,1,1,1,1,1,1,1,1,1,1,1,1,1,1,1,1,1,1,1,1,1,1,1,1,1,1,1,
1,1,1,1,1,1,1,1,4),(-0.000359643560771195,0.0826961570524529),(11.6143855724915,
12.1066224675668,12.598175811328,13.5812824988505,14.5643891863729,15.5474958738954,
16.5306025614178,17.5137092489403,18.4968159364627,19.4799226239851,20.4630293115076,
21.44613599903,22.4292426865525,23.4123493740749,24.3954560615974,25.3785627491198,
26.3616694366423,27.3447761241647,28.3278828116872,29.3109894992096,30.294096186732,
31.2772028742545,32.2603095617769,33.2434162492994,34.2265229368218,35.2096296243443,
36.1927363118667,37.1758429993892,38.1589496869116,39.142056374434,40.1251630619565,
41.1082697494789,42.0913764370014,43.0744831245238,44.0575898120463,45.0406964995687,
46.0238031870912,47.0069098746136,47.9900165621361,48.9731232496585,49.956229937181,
50.9393366247034,51.9224433122258,52.9055499997483,53.3971033435095,53.8886566872707),
 .UNSPECIFIED.);
#3611=B_SPLINE_SURFACE_WITH_KNOTS('',3,3,((#26503,#26504,#26505,#26506,
#26507,#26508,#26509,#26510,#26511,#26512,#26513,#26514,#26515,#26516,#26517,
#26518,#26519,#26520,#26521,#26522,#26523,#26524,#26525,#26526,#26527,#26528,
#26529,#26530,#26531,#26532,#26533,#26534,#26535,#26536,#26537,#26538,#26539,
#26540,#26541,#26542,#26543,#26544,#26545,#26546,#26547,#26548,#26549,#26550,
#26551,#26552,#26553,#26554,#26555,#26556,#26557,#26558,#26559,#26560,#26561,
#26562,#26563,#26564,#26565,#26566,#26567,#26568,#26569,#26570,#26571,#26572,
#26573,#26574,#26575,#26576,#26577,#26578,#26579,#26580,#26581,#26582,#26583,
#26584,#26585,#26586,#26587,#26588,#26589,#26590,#26591),(#26592,#26593,
#26594,#26595,#26596,#26597,#26598,#26599,#26600,#26601,#26602,#26603,#26604,
#26605,#26606,#26607,#26608,#26609,#26610,#26611,#26612,#26613,#26614,#26615,
#26616,#26617,#26618,#26619,#26620,#26621,#26622,#26623,#26624,#26625,#26626,
#26627,#26628,#26629,#26630,#26631,#26632,#26633,#26634,#26635,#26636,#26637,
#26638,#26639,#26640,#26641,#26642,#26643,#26644,#26645,#26646,#26647,#26648,
#26649,#26650,#26651,#26652,#26653,#26654,#26655,#26656,#26657,#26658,#26659,
#26660,#26661,#26662,#26663,#26664,#26665,#26666,#26667,#26668,#26669,#26670,
#26671,#26672,#26673,#26674,#26675,#26676,#26677,#26678,#26679,#26680),
(#26681,#26682,#26683,#26684,#26685,#26686,#26687,#26688,#26689,#26690,
#26691,#26692,#26693,#26694,#26695,#26696,#26697,#26698,#26699,#26700,#26701,
#26702,#26703,#26704,#26705,#26706,#26707,#26708,#26709,#26710,#26711,#26712,
#26713,#26714,#26715,#26716,#26717,#26718,#26719,#26720,#26721,#26722,#26723,
#26724,#26725,#26726,#26727,#26728,#26729,#26730,#26731,#26732,#26733,#26734,
#26735,#26736,#26737,#26738,#26739,#26740,#26741,#26742,#26743,#26744,#26745,
#26746,#26747,#26748,#26749,#26750,#26751,#26752,#26753,#26754,#26755,#26756,
#26757,#26758,#26759,#26760,#26761,#26762,#26763,#26764,#26765,#26766,#26767,
#26768,#26769),(#26770,#26771,#26772,#26773,#26774,#26775,#26776,#26777,
#26778,#26779,#26780,#26781,#26782,#26783,#26784,#26785,#26786,#26787,#26788,
#26789,#26790,#26791,#26792,#26793,#26794,#26795,#26796,#26797,#26798,#26799,
#26800,#26801,#26802,#26803,#26804,#26805,#26806,#26807,#26808,#26809,#26810,
#26811,#26812,#26813,#26814,#26815,#26816,#26817,#26818,#26819,#26820,#26821,
#26822,#26823,#26824,#26825,#26826,#26827,#26828,#26829,#26830,#26831,#26832,
#26833,#26834,#26835,#26836,#26837,#26838,#26839,#26840,#26841,#26842,#26843,
#26844,#26845,#26846,#26847,#26848,#26849,#26850,#26851,#26852,#26853,#26854,
#26855,#26856,#26857,#26858)),.UNSPECIFIED.,.F.,.F.,.F.,(4,4),(4,1,1,1,
1,1,1,1,1,1,1,1,1,1,1,1,1,1,1,1,1,1,1,1,1,1,1,1,1,1,1,1,1,1,1,1,1,1,1,1,
1,1,1,1,1,1,1,1,1,1,1,1,1,1,1,1,1,1,1,1,1,1,1,1,1,1,1,1,1,1,1,1,1,1,1,1,
1,1,1,1,1,1,1,1,1,1,4),(-0.000803760615569271,0.050103355208433),(13.3936548749541,
14.3924503130856,15.3906450173941,16.3888397217026,17.3870344260111,18.3852291303196,
19.3834238346281,20.3816185389366,21.3798132432451,22.3780079475536,23.3762026518621,
24.3743973561706,25.3725920604791,26.3707867647876,27.3689814690961,28.3671761734046,
29.365370877713,30.3635655820215,31.36176028633,32.3599549906385,33.358149694947,
34.3563443992555,35.354539103564,36.3527338078725,37.350928512181,38.3491232164895,
39.347317920798,40.3455126251065,41.343707329415,42.3419020337235,43.340096738032,
44.3382914423405,45.336486146649,46.3346808509575,47.332875555266,48.3310702595745,
49.329264963883,50.3274596681915,51.3256543725,52.3238490768085,53.322043781117,
54.3202384854255,55.318433189734,56.3166278940425,57.314822598351,58.3130173026595,
59.311212006968,60.3094067112765,61.307601415585,62.3057961198935,63.303990824202,
64.3021855285105,65.300380232819,66.2985749371275,67.296769641436,68.2949643457444,
69.2931590500529,70.2913537543614,71.2895484586699,72.2877431629784,73.2859378672869,
74.2841325715954,75.2823272759039,76.2805219802124,77.2787166845209,78.2769113888294,
79.2751060931379,80.2733007974464,81.2714955017549,82.2696902060634,83.2678849103719,
84.2660796146804,85.2642743189889,86.2624690232974,87.2606637276059,88.2588584319144,
89.2570531362229,90.2552478405314,91.2534425448399,92.2516372491484,93.2498319534569,
94.2480266577654,95.2462213620739,96.2444160663824,97.2426107706909,98.2408054749994,
99.2393733588525),.UNSPECIFIED.);
#3612=B_SPLINE_SURFACE_WITH_KNOTS('',3,3,((#27117,#27118,#27119,#27120,
#27121,#27122,#27123,#27124,#27125,#27126,#27127,#27128,#27129,#27130,#27131,
#27132,#27133,#27134,#27135,#27136,#27137,#27138,#27139,#27140,#27141,#27142,
#27143,#27144,#27145,#27146,#27147,#27148,#27149,#27150,#27151,#27152,#27153,
#27154,#27155,#27156,#27157,#27158,#27159,#27160,#27161,#27162,#27163,#27164,
#27165,#27166,#27167,#27168,#27169,#27170,#27171,#27172,#27173,#27174,#27175,
#27176,#27177,#27178,#27179,#27180,#27181,#27182,#27183,#27184,#27185,#27186,
#27187,#27188,#27189,#27190,#27191,#27192,#27193,#27194,#27195,#27196,#27197,
#27198,#27199,#27200,#27201,#27202,#27203,#27204,#27205),(#27206,#27207,
#27208,#27209,#27210,#27211,#27212,#27213,#27214,#27215,#27216,#27217,#27218,
#27219,#27220,#27221,#27222,#27223,#27224,#27225,#27226,#27227,#27228,#27229,
#27230,#27231,#27232,#27233,#27234,#27235,#27236,#27237,#27238,#27239,#27240,
#27241,#27242,#27243,#27244,#27245,#27246,#27247,#27248,#27249,#27250,#27251,
#27252,#27253,#27254,#27255,#27256,#27257,#27258,#27259,#27260,#27261,#27262,
#27263,#27264,#27265,#27266,#27267,#27268,#27269,#27270,#27271,#27272,#27273,
#27274,#27275,#27276,#27277,#27278,#27279,#27280,#27281,#27282,#27283,#27284,
#27285,#27286,#27287,#27288,#27289,#27290,#27291,#27292,#27293,#27294),
(#27295,#27296,#27297,#27298,#27299,#27300,#27301,#27302,#27303,#27304,
#27305,#27306,#27307,#27308,#27309,#27310,#27311,#27312,#27313,#27314,#27315,
#27316,#27317,#27318,#27319,#27320,#27321,#27322,#27323,#27324,#27325,#27326,
#27327,#27328,#27329,#27330,#27331,#27332,#27333,#27334,#27335,#27336,#27337,
#27338,#27339,#27340,#27341,#27342,#27343,#27344,#27345,#27346,#27347,#27348,
#27349,#27350,#27351,#27352,#27353,#27354,#27355,#27356,#27357,#27358,#27359,
#27360,#27361,#27362,#27363,#27364,#27365,#27366,#27367,#27368,#27369,#27370,
#27371,#27372,#27373,#27374,#27375,#27376,#27377,#27378,#27379,#27380,#27381,
#27382,#27383),(#27384,#27385,#27386,#27387,#27388,#27389,#27390,#27391,
#27392,#27393,#27394,#27395,#27396,#27397,#27398,#27399,#27400,#27401,#27402,
#27403,#27404,#27405,#27406,#27407,#27408,#27409,#27410,#27411,#27412,#27413,
#27414,#27415,#27416,#27417,#27418,#27419,#27420,#27421,#27422,#27423,#27424,
#27425,#27426,#27427,#27428,#27429,#27430,#27431,#27432,#27433,#27434,#27435,
#27436,#27437,#27438,#27439,#27440,#27441,#27442,#27443,#27444,#27445,#27446,
#27447,#27448,#27449,#27450,#27451,#27452,#27453,#27454,#27455,#27456,#27457,
#27458,#27459,#27460,#27461,#27462,#27463,#27464,#27465,#27466,#27467,#27468,
#27469,#27470,#27471,#27472)),.UNSPECIFIED.,.F.,.F.,.F.,(4,4),(4,1,1,1,
1,1,1,1,1,1,1,1,1,1,1,1,1,1,1,1,1,1,1,1,1,1,1,1,1,1,1,1,1,1,1,1,1,1,1,1,
1,1,1,1,1,1,1,1,1,1,1,1,1,1,1,1,1,1,1,1,1,1,1,1,1,1,1,1,1,1,1,1,1,1,1,1,
1,1,1,1,1,1,1,1,1,1,4),(-0.000630172471168558,0.0497654761150975),(16.7016191235447,
17.7001869884391,18.6983816927476,19.6965763970561,20.6947711013646,21.6929658056731,
22.6911605099816,23.6893552142901,24.6875499185986,25.6857446229071,26.6839393272156,
27.6821340315241,28.6803287358326,29.6785234401411,30.6767181444496,31.6749128487581,
32.6731075530666,33.6713022573751,34.6694969616836,35.6676916659921,36.6658863703006,
37.6640810746091,38.6622757789176,39.6604704832261,40.6586651875346,41.6568598918431,
42.6550545961516,43.65324930046,44.6514440047685,45.6496387090771,46.6478334133855,
47.646028117694,48.6442228220025,49.642417526311,50.6406122306195,51.638806934928,
52.6370016392365,53.635196343545,54.6333910478535,55.631585752162,56.6297804564705,
57.627975160779,58.6261698650875,59.624364569396,60.6225592737045,61.620753978013,
62.6189486823215,63.61714338663,64.6153380909385,65.613532795247,66.6117274995555,
67.609922203864,68.6081169081725,69.606311612481,70.6045063167895,71.602701021098,
72.6008957254065,73.599090429715,74.5972851340235,75.595479838332,76.5936745426405,
77.591869246949,78.5900639512575,79.588258655566,80.5864533598745,81.584648064183,
82.5828427684915,83.5810374728,84.5792321771085,85.577426881417,86.5756215857255,
87.573816290034,88.5720109943425,89.570205698651,90.5684004029595,91.566595107268,
92.5647898115765,93.562984515885,94.5611792201935,95.559373924502,96.5575686288105,
97.555763333119,98.5539580374275,99.552152741736,100.550347446044,101.548542150353,
102.547367027132),.UNSPECIFIED.);
#3613=ADVANCED_FACE('',(#438),#3575,.T.);
#3614=ADVANCED_FACE('',(#439),#344,.F.);
#3615=ADVANCED_FACE('',(#440),#3576,.T.);
#3616=ADVANCED_FACE('',(#441),#345,.F.);
#3617=ADVANCED_FACE('',(#442),#163,.T.);
#3618=ADVANCED_FACE('',(#443),#164,.T.);
#3619=ADVANCED_FACE('',(#444),#165,.T.);
#3620=ADVANCED_FACE('',(#445),#166,.T.);
#3621=ADVANCED_FACE('',(#446),#167,.T.);
#3622=ADVANCED_FACE('',(#447),#168,.T.);
#3623=ADVANCED_FACE('',(#448,#128),#169,.T.);
#3624=ADVANCED_FACE('',(#449,#129),#170,.F.);
#3625=ADVANCED_FACE('',(#450),#346,.F.);
#3626=ADVANCED_FACE('',(#451,#130),#347,.F.);
#3627=ADVANCED_FACE('',(#452,#131),#171,.T.);
#3628=ADVANCED_FACE('',(#453),#70,.T.);
#3629=ADVANCED_FACE('',(#454,#132),#348,.T.);
#3630=ADVANCED_FACE('',(#455),#71,.T.);
#3631=ADVANCED_FACE('',(#456,#133),#172,.T.);
#3632=ADVANCED_FACE('',(#457),#349,.F.);
#3633=ADVANCED_FACE('',(#458,#134),#173,.T.);
#3634=ADVANCED_FACE('',(#459),#350,.F.);
#3635=ADVANCED_FACE('',(#460,#135),#174,.T.);
#3636=ADVANCED_FACE('',(#461),#3577,.T.);
#3637=ADVANCED_FACE('',(#462),#351,.F.);
#3638=ADVANCED_FACE('',(#463),#3578,.T.);
#3639=ADVANCED_FACE('',(#464),#352,.F.);
#3640=ADVANCED_FACE('',(#465),#175,.T.);
#3641=ADVANCED_FACE('',(#466),#176,.T.);
#3642=ADVANCED_FACE('',(#467),#177,.T.);
#3643=ADVANCED_FACE('',(#468),#178,.T.);
#3644=ADVANCED_FACE('',(#469),#179,.T.);
#3645=ADVANCED_FACE('',(#470),#180,.T.);
#3646=ADVANCED_FACE('',(#471,#136),#181,.T.);
#3647=ADVANCED_FACE('',(#472,#137),#182,.F.);
#3648=ADVANCED_FACE('',(#473),#183,.F.);
#3649=ADVANCED_FACE('',(#474),#184,.F.);
#3650=ADVANCED_FACE('',(#475),#353,.T.);
#3651=ADVANCED_FACE('',(#476),#354,.T.);
#3652=ADVANCED_FACE('',(#477),#355,.T.);
#3653=ADVANCED_FACE('',(#478),#356,.T.);
#3654=ADVANCED_FACE('',(#479),#357,.T.);
#3655=ADVANCED_FACE('',(#480),#358,.T.);
#3656=ADVANCED_FACE('',(#481),#359,.T.);
#3657=ADVANCED_FACE('',(#482),#360,.T.);
#3658=ADVANCED_FACE('',(#483),#361,.T.);
#3659=ADVANCED_FACE('',(#484),#362,.T.);
#3660=ADVANCED_FACE('',(#485),#363,.T.);
#3661=ADVANCED_FACE('',(#486),#364,.T.);
#3662=ADVANCED_FACE('',(#487),#365,.T.);
#3663=ADVANCED_FACE('',(#488),#366,.T.);
#3664=ADVANCED_FACE('',(#489),#3579,.F.);
#3665=ADVANCED_FACE('',(#490),#3580,.F.);
#3666=ADVANCED_FACE('',(#491),#3581,.F.);
#3667=ADVANCED_FACE('',(#492),#3582,.F.);
#3668=ADVANCED_FACE('',(#493),#3583,.F.);
#3669=ADVANCED_FACE('',(#494),#3584,.F.);
#3670=ADVANCED_FACE('',(#495),#3585,.F.);
#3671=ADVANCED_FACE('',(#496),#3586,.F.);
#3672=ADVANCED_FACE('',(#497),#3587,.F.);
#3673=ADVANCED_FACE('',(#498),#3588,.F.);
#3674=ADVANCED_FACE('',(#499),#3589,.F.);
#3675=ADVANCED_FACE('',(#500),#3590,.F.);
#3676=ADVANCED_FACE('',(#501),#3591,.F.);
#3677=ADVANCED_FACE('',(#502),#3592,.F.);
#3678=ADVANCED_FACE('',(#503),#185,.T.);
#3679=ADVANCED_FACE('',(#504),#367,.T.);
#3680=ADVANCED_FACE('',(#505),#368,.T.);
#3681=ADVANCED_FACE('',(#506),#369,.T.);
#3682=ADVANCED_FACE('',(#507),#370,.T.);
#3683=ADVANCED_FACE('',(#508),#371,.T.);
#3684=ADVANCED_FACE('',(#509),#372,.T.);
#3685=ADVANCED_FACE('',(#510),#373,.T.);
#3686=ADVANCED_FACE('',(#511),#374,.T.);
#3687=ADVANCED_FACE('',(#512),#375,.T.);
#3688=ADVANCED_FACE('',(#513),#376,.T.);
#3689=ADVANCED_FACE('',(#514),#377,.T.);
#3690=ADVANCED_FACE('',(#515),#378,.T.);
#3691=ADVANCED_FACE('',(#516),#379,.T.);
#3692=ADVANCED_FACE('',(#517),#380,.T.);
#3693=ADVANCED_FACE('',(#518),#3593,.F.);
#3694=ADVANCED_FACE('',(#519),#3594,.F.);
#3695=ADVANCED_FACE('',(#520),#3595,.F.);
#3696=ADVANCED_FACE('',(#521),#3596,.F.);
#3697=ADVANCED_FACE('',(#522),#3597,.F.);
#3698=ADVANCED_FACE('',(#523),#3598,.F.);
#3699=ADVANCED_FACE('',(#524),#3599,.F.);
#3700=ADVANCED_FACE('',(#525),#3600,.F.);
#3701=ADVANCED_FACE('',(#526),#3601,.F.);
#3702=ADVANCED_FACE('',(#527),#3602,.F.);
#3703=ADVANCED_FACE('',(#528),#3603,.F.);
#3704=ADVANCED_FACE('',(#529),#3604,.F.);
#3705=ADVANCED_FACE('',(#530),#3605,.F.);
#3706=ADVANCED_FACE('',(#531),#3606,.F.);
#3707=ADVANCED_FACE('',(#532),#381,.T.);
#3708=ADVANCED_FACE('',(#533,#138),#186,.T.);
#3709=ADVANCED_FACE('',(#534),#187,.F.);
#3710=ADVANCED_FACE('',(#535),#51,.T.);
#3711=ADVANCED_FACE('',(#536),#72,.T.);
#3712=ADVANCED_FACE('',(#537),#188,.T.);
#3713=ADVANCED_FACE('',(#538),#52,.T.);
#3714=ADVANCED_FACE('',(#539),#189,.T.);
#3715=ADVANCED_FACE('',(#540),#382,.T.);
#3716=ADVANCED_FACE('',(#541),#383,.T.);
#3717=ADVANCED_FACE('',(#542),#384,.T.);
#3718=ADVANCED_FACE('',(#543),#385,.T.);
#3719=ADVANCED_FACE('',(#544),#386,.T.);
#3720=ADVANCED_FACE('',(#545),#387,.T.);
#3721=ADVANCED_FACE('',(#546),#388,.T.);
#3722=ADVANCED_FACE('',(#547),#389,.T.);
#3723=ADVANCED_FACE('',(#548),#3607,.T.);
#3724=ADVANCED_FACE('',(#549),#390,.F.);
#3725=ADVANCED_FACE('',(#550),#3608,.T.);
#3726=ADVANCED_FACE('',(#551),#190,.F.);
#3727=ADVANCED_FACE('',(#552),#391,.F.);
#3728=ADVANCED_FACE('',(#553),#3609,.F.);
#3729=ADVANCED_FACE('',(#554),#3610,.F.);
#3730=ADVANCED_FACE('',(#555),#392,.T.);
#3731=ADVANCED_FACE('',(#556,#139),#191,.T.);
#3732=ADVANCED_FACE('',(#557,#140),#192,.T.);
#3733=ADVANCED_FACE('',(#558,#141),#193,.F.);
#3734=ADVANCED_FACE('',(#559),#73,.T.);
#3735=ADVANCED_FACE('',(#560,#142),#194,.F.);
#3736=ADVANCED_FACE('',(#561),#393,.T.);
#3737=ADVANCED_FACE('',(#562),#394,.F.);
#3738=ADVANCED_FACE('',(#563),#395,.F.);
#3739=ADVANCED_FACE('',(#564,#143),#195,.T.);
#3740=ADVANCED_FACE('',(#565),#74,.T.);
#3741=ADVANCED_FACE('',(#566,#144),#396,.T.);
#3742=ADVANCED_FACE('',(#567),#75,.T.);
#3743=ADVANCED_FACE('',(#568),#76,.T.);
#3744=ADVANCED_FACE('',(#569),#77,.F.);
#3745=ADVANCED_FACE('',(#570),#397,.F.);
#3746=ADVANCED_FACE('',(#571),#78,.F.);
#3747=ADVANCED_FACE('',(#572,#145),#196,.T.);
#3748=ADVANCED_FACE('',(#573),#398,.F.);
#3749=ADVANCED_FACE('',(#574,#146),#197,.T.);
#3750=ADVANCED_FACE('',(#575),#79,.F.);
#3751=ADVANCED_FACE('',(#576),#399,.F.);
#3752=ADVANCED_FACE('',(#577),#80,.F.);
#3753=ADVANCED_FACE('',(#578),#400,.F.);
#3754=ADVANCED_FACE('',(#579),#81,.F.);
#3755=ADVANCED_FACE('',(#580,#147),#198,.T.);
#3756=ADVANCED_FACE('',(#581),#401,.F.);
#3757=ADVANCED_FACE('',(#582,#148),#199,.T.);
#3758=ADVANCED_FACE('',(#583,#149),#402,.F.);
#3759=ADVANCED_FACE('',(#584,#150),#200,.T.);
#3760=ADVANCED_FACE('',(#585),#53,.T.);
#3761=ADVANCED_FACE('',(#586),#82,.T.);
#3762=ADVANCED_FACE('',(#587),#201,.T.);
#3763=ADVANCED_FACE('',(#588),#54,.T.);
#3764=ADVANCED_FACE('',(#589),#202,.T.);
#3765=ADVANCED_FACE('',(#590,#151),#403,.T.);
#3766=ADVANCED_FACE('',(#591),#404,.T.);
#3767=ADVANCED_FACE('',(#592),#405,.T.);
#3768=ADVANCED_FACE('',(#593),#406,.T.);
#3769=ADVANCED_FACE('',(#594),#407,.T.);
#3770=ADVANCED_FACE('',(#595),#408,.T.);
#3771=ADVANCED_FACE('',(#596),#409,.T.);
#3772=ADVANCED_FACE('',(#597),#410,.T.);
#3773=ADVANCED_FACE('',(#598),#411,.T.);
#3774=ADVANCED_FACE('',(#599),#412,.T.);
#3775=ADVANCED_FACE('',(#600),#413,.T.);
#3776=ADVANCED_FACE('',(#601),#414,.T.);
#3777=ADVANCED_FACE('',(#602),#415,.T.);
#3778=ADVANCED_FACE('',(#603),#416,.T.);
#3779=ADVANCED_FACE('',(#604),#417,.T.);
#3780=ADVANCED_FACE('',(#605),#418,.T.);
#3781=ADVANCED_FACE('',(#606),#419,.T.);
#3782=ADVANCED_FACE('',(#607),#420,.T.);
#3783=ADVANCED_FACE('',(#608),#421,.T.);
#3784=ADVANCED_FACE('',(#609),#422,.T.);
#3785=ADVANCED_FACE('',(#610),#423,.T.);
#3786=ADVANCED_FACE('',(#611),#424,.T.);
#3787=ADVANCED_FACE('',(#612),#425,.T.);
#3788=ADVANCED_FACE('',(#613),#426,.T.);
#3789=ADVANCED_FACE('',(#614),#427,.T.);
#3790=ADVANCED_FACE('',(#615),#428,.T.);
#3791=ADVANCED_FACE('',(#616),#429,.T.);
#3792=ADVANCED_FACE('',(#617),#430,.F.);
#3793=ADVANCED_FACE('',(#618),#203,.T.);
#3794=ADVANCED_FACE('',(#619),#431,.T.);
#3795=ADVANCED_FACE('',(#620,#152),#204,.T.);
#3796=ADVANCED_FACE('',(#621),#55,.T.);
#3797=ADVANCED_FACE('',(#622),#83,.T.);
#3798=ADVANCED_FACE('',(#623),#56,.T.);
#3799=ADVANCED_FACE('',(#624,#153),#205,.T.);
#3800=ADVANCED_FACE('',(#625),#3611,.F.);
#3801=ADVANCED_FACE('',(#626),#206,.T.);
#3802=ADVANCED_FACE('',(#627),#3612,.F.);
#3803=ADVANCED_FACE('',(#628),#207,.T.);
#3804=ADVANCED_FACE('',(#629),#57,.T.);
#3805=ADVANCED_FACE('',(#630),#432,.T.);
#3806=ADVANCED_FACE('',(#631,#154),#208,.T.);
#3807=ADVANCED_FACE('',(#632),#58,.T.);
#3808=ADVANCED_FACE('',(#633),#84,.T.);
#3809=ADVANCED_FACE('',(#634,#155),#209,.T.);
#3810=ADVANCED_FACE('',(#635),#59,.T.);
#3811=ADVANCED_FACE('',(#636,#156),#210,.T.);
#3812=ADVANCED_FACE('',(#637),#60,.T.);
#3813=ADVANCED_FACE('',(#638),#85,.T.);
#3814=ADVANCED_FACE('',(#639,#157),#211,.T.);
#3815=ADVANCED_FACE('',(#640),#61,.T.);
#3816=ADVANCED_FACE('',(#641),#62,.T.);
#3817=ADVANCED_FACE('',(#642),#86,.T.);
#3818=ADVANCED_FACE('',(#643),#63,.T.);
#3819=ADVANCED_FACE('',(#644,#158),#212,.T.);
#3820=ADVANCED_FACE('',(#645),#64,.T.);
#3821=ADVANCED_FACE('',(#646),#87,.T.);
#3822=ADVANCED_FACE('',(#647,#159),#213,.T.);
#3823=ADVANCED_FACE('',(#648),#65,.T.);
#3824=ADVANCED_FACE('',(#649,#160),#214,.T.);
#3825=ADVANCED_FACE('',(#650),#66,.T.);
#3826=ADVANCED_FACE('',(#651),#215,.T.);
#3827=ADVANCED_FACE('',(#652),#433,.T.);
#3828=ADVANCED_FACE('',(#653),#434,.T.);
#3829=ADVANCED_FACE('',(#654),#435,.T.);
#3830=ADVANCED_FACE('',(#655),#436,.T.);
#3831=ADVANCED_FACE('',(#656,#161),#216,.T.);
#3832=ADVANCED_FACE('',(#657),#437,.F.);
#3833=ADVANCED_FACE('',(#658,#162),#217,.T.);
#3834=CLOSED_SHELL('',(#3613,#3614,#3615,#3616,#3617,#3618,#3619,#3620,
#3621,#3622,#3623,#3624));
#3835=CLOSED_SHELL('',(#3625,#3626,#3627,#3628,#3629,#3630,#3631,#3632,
#3633,#3634,#3635));
#3836=CLOSED_SHELL('',(#3636,#3637,#3638,#3639,#3640,#3641,#3642,#3643,
#3644,#3645,#3646,#3647));
#3837=CLOSED_SHELL('',(#3648,#3649,#3650,#3651,#3652,#3653,#3654,#3655,
#3656,#3657,#3658,#3659,#3660,#3661,#3662,#3663,#3664,#3665,#3666,#3667,
#3668,#3669,#3670,#3671,#3672,#3673,#3674,#3675,#3676,#3677,#3678,#3679,
#3680,#3681,#3682,#3683,#3684,#3685,#3686,#3687,#3688,#3689,#3690,#3691,
#3692,#3693,#3694,#3695,#3696,#3697,#3698,#3699,#3700,#3701,#3702,#3703,
#3704,#3705,#3706,#3707,#3708,#3709));
#3838=CLOSED_SHELL('',(#3710,#3711,#3712,#3713,#3714));
#3839=CLOSED_SHELL('',(#3715,#3716,#3717,#3718,#3719,#3720,#3721,#3722,
#3723,#3724,#3725,#3726,#3727,#3728,#3729,#3730,#3731,#3732,#3733));
#3840=CLOSED_SHELL('',(#3734,#3735,#3736,#3737,#3738,#3739,#3740,#3741,
#3742,#3743,#3744,#3745,#3746,#3747,#3748,#3749,#3750,#3751,#3752,#3753,
#3754,#3755,#3756,#3757,#3758,#3759));
#3841=CLOSED_SHELL('',(#3760,#3761,#3762,#3763,#3764));
#3842=CLOSED_SHELL('',(#3765,#3766,#3767,#3768,#3769,#3770,#3771,#3772,
#3773,#3774,#3775,#3776,#3777,#3778,#3779,#3780,#3781,#3782,#3783,#3784,
#3785,#3786,#3787,#3788,#3789,#3790,#3791,#3792,#3793,#3794,#3795,#3796,
#3797,#3798,#3799,#3800,#3801,#3802,#3803,#3804,#3805,#3806,#3807,#3808,
#3809,#3810,#3811,#3812,#3813,#3814,#3815,#3816,#3817,#3818,#3819,#3820,
#3821,#3822,#3823,#3824,#3825,#3826,#3827,#3828,#3829));
#3843=CLOSED_SHELL('',(#3830,#3831,#3832,#3833));
#3844=DERIVED_UNIT_ELEMENT(#3864,1.);
#3845=DERIVED_UNIT_ELEMENT(#27709,-3.);
#3846=DERIVED_UNIT_ELEMENT(#3864,1.);
#3847=DERIVED_UNIT_ELEMENT(#27709,-3.);
#3848=DERIVED_UNIT_ELEMENT(#3864,1.);
#3849=DERIVED_UNIT_ELEMENT(#27709,-3.);
#3850=DERIVED_UNIT_ELEMENT(#3864,1.);
#3851=DERIVED_UNIT_ELEMENT(#27709,-3.);
#3852=DERIVED_UNIT_ELEMENT(#3864,1.);
#3853=DERIVED_UNIT_ELEMENT(#27709,-3.);
#3854=DERIVED_UNIT_ELEMENT(#3864,1.);
#3855=DERIVED_UNIT_ELEMENT(#27709,-3.);
#3856=DERIVED_UNIT_ELEMENT(#3864,1.);
#3857=DERIVED_UNIT_ELEMENT(#27709,-3.);
#3858=DERIVED_UNIT_ELEMENT(#3864,1.);
#3859=DERIVED_UNIT_ELEMENT(#27709,-3.);
#3860=DERIVED_UNIT_ELEMENT(#3864,1.);
#3861=DERIVED_UNIT_ELEMENT(#27709,-3.);
#3862=DERIVED_UNIT_ELEMENT(#3864,1.);
#3863=DERIVED_UNIT_ELEMENT(#27709,-3.);
#3864=(
MASS_UNIT()
NAMED_UNIT(*)
SI_UNIT(.KILO.,.GRAM.)
);
#3865=DERIVED_UNIT((#3844,#3845));
#3866=DERIVED_UNIT((#3846,#3847));
#3867=DERIVED_UNIT((#3848,#3849));
#3868=DERIVED_UNIT((#3850,#3851));
#3869=DERIVED_UNIT((#3852,#3853));
#3870=DERIVED_UNIT((#3854,#3855));
#3871=DERIVED_UNIT((#3856,#3857));
#3872=DERIVED_UNIT((#3858,#3859));
#3873=DERIVED_UNIT((#3860,#3861));
#3874=DERIVED_UNIT((#3862,#3863));
#3875=MEASURE_REPRESENTATION_ITEM('density measure',
POSITIVE_RATIO_MEASURE(7850.),#3865);
#3876=MEASURE_REPRESENTATION_ITEM('density measure',
POSITIVE_RATIO_MEASURE(7850.),#3866);
#3877=MEASURE_REPRESENTATION_ITEM('density measure',
POSITIVE_RATIO_MEASURE(7850.),#3867);
#3878=MEASURE_REPRESENTATION_ITEM('density measure',
POSITIVE_RATIO_MEASURE(7850.),#3868);
#3879=MEASURE_REPRESENTATION_ITEM('density measure',
POSITIVE_RATIO_MEASURE(7850.),#3869);
#3880=MEASURE_REPRESENTATION_ITEM('density measure',
POSITIVE_RATIO_MEASURE(7850.),#3870);
#3881=MEASURE_REPRESENTATION_ITEM('density measure',
POSITIVE_RATIO_MEASURE(7850.),#3871);
#3882=MEASURE_REPRESENTATION_ITEM('density measure',
POSITIVE_RATIO_MEASURE(7850.),#3872);
#3883=MEASURE_REPRESENTATION_ITEM('density measure',
POSITIVE_RATIO_MEASURE(7850.),#3873);
#3884=MEASURE_REPRESENTATION_ITEM('density measure',
POSITIVE_RATIO_MEASURE(7850.),#3874);
#3885=PROPERTY_DEFINITION_REPRESENTATION(#3935,#3905);
#3886=PROPERTY_DEFINITION_REPRESENTATION(#3936,#3906);
#3887=PROPERTY_DEFINITION_REPRESENTATION(#3937,#3907);
#3888=PROPERTY_DEFINITION_REPRESENTATION(#3938,#3908);
#3889=PROPERTY_DEFINITION_REPRESENTATION(#3939,#3909);
#3890=PROPERTY_DEFINITION_REPRESENTATION(#3940,#3910);
#3891=PROPERTY_DEFINITION_REPRESENTATION(#3941,#3911);
#3892=PROPERTY_DEFINITION_REPRESENTATION(#3942,#3912);
#3893=PROPERTY_DEFINITION_REPRESENTATION(#3943,#3913);
#3894=PROPERTY_DEFINITION_REPRESENTATION(#3944,#3914);
#3895=PROPERTY_DEFINITION_REPRESENTATION(#3945,#3915);
#3896=PROPERTY_DEFINITION_REPRESENTATION(#3946,#3916);
#3897=PROPERTY_DEFINITION_REPRESENTATION(#3947,#3917);
#3898=PROPERTY_DEFINITION_REPRESENTATION(#3948,#3918);
#3899=PROPERTY_DEFINITION_REPRESENTATION(#3949,#3919);
#3900=PROPERTY_DEFINITION_REPRESENTATION(#3950,#3920);
#3901=PROPERTY_DEFINITION_REPRESENTATION(#3951,#3921);
#3902=PROPERTY_DEFINITION_REPRESENTATION(#3952,#3922);
#3903=PROPERTY_DEFINITION_REPRESENTATION(#3953,#3923);
#3904=PROPERTY_DEFINITION_REPRESENTATION(#3954,#3924);
#3905=REPRESENTATION('material name',(#3925),#27697);
#3906=REPRESENTATION('density',(#3875),#27697);
#3907=REPRESENTATION('material name',(#3926),#27698);
#3908=REPRESENTATION('density',(#3876),#27698);
#3909=REPRESENTATION('material name',(#3927),#27699);
#3910=REPRESENTATION('density',(#3877),#27699);
#3911=REPRESENTATION('material name',(#3928),#27700);
#3912=REPRESENTATION('density',(#3878),#27700);
#3913=REPRESENTATION('material name',(#3929),#27701);
#3914=REPRESENTATION('density',(#3879),#27701);
#3915=REPRESENTATION('material name',(#3930),#27702);
#3916=REPRESENTATION('density',(#3880),#27702);
#3917=REPRESENTATION('material name',(#3931),#27703);
#3918=REPRESENTATION('density',(#3881),#27703);
#3919=REPRESENTATION('material name',(#3932),#27704);
#3920=REPRESENTATION('density',(#3882),#27704);
#3921=REPRESENTATION('material name',(#3933),#27705);
#3922=REPRESENTATION('density',(#3883),#27705);
#3923=REPRESENTATION('material name',(#3934),#27706);
#3924=REPRESENTATION('density',(#3884),#27706);
#3925=DESCRIPTIVE_REPRESENTATION_ITEM('Steel','Steel');
#3926=DESCRIPTIVE_REPRESENTATION_ITEM('Steel','Steel');
#3927=DESCRIPTIVE_REPRESENTATION_ITEM('Steel','Steel');
#3928=DESCRIPTIVE_REPRESENTATION_ITEM('Steel','Steel');
#3929=DESCRIPTIVE_REPRESENTATION_ITEM('Steel','Steel');
#3930=DESCRIPTIVE_REPRESENTATION_ITEM('Steel','Steel');
#3931=DESCRIPTIVE_REPRESENTATION_ITEM('Steel','Steel');
#3932=DESCRIPTIVE_REPRESENTATION_ITEM('Steel','Steel');
#3933=DESCRIPTIVE_REPRESENTATION_ITEM('Steel','Steel');
#3934=DESCRIPTIVE_REPRESENTATION_ITEM('Steel','Steel');
#3935=PROPERTY_DEFINITION('material property','material name',#27757);
#3936=PROPERTY_DEFINITION('material property','density of part',#27757);
#3937=PROPERTY_DEFINITION('material property','material name',#27758);
#3938=PROPERTY_DEFINITION('material property','density of part',#27758);
#3939=PROPERTY_DEFINITION('material property','material name',#27759);
#3940=PROPERTY_DEFINITION('material property','density of part',#27759);
#3941=PROPERTY_DEFINITION('material property','material name',#27760);
#3942=PROPERTY_DEFINITION('material property','density of part',#27760);
#3943=PROPERTY_DEFINITION('material property','material name',#27761);
#3944=PROPERTY_DEFINITION('material property','density of part',#27761);
#3945=PROPERTY_DEFINITION('material property','material name',#27762);
#3946=PROPERTY_DEFINITION('material property','density of part',#27762);
#3947=PROPERTY_DEFINITION('material property','material name',#27763);
#3948=PROPERTY_DEFINITION('material property','density of part',#27763);
#3949=PROPERTY_DEFINITION('material property','material name',#27764);
#3950=PROPERTY_DEFINITION('material property','density of part',#27764);
#3951=PROPERTY_DEFINITION('material property','material name',#27765);
#3952=PROPERTY_DEFINITION('material property','density of part',#27765);
#3953=PROPERTY_DEFINITION('material property','material name',#27766);
#3954=PROPERTY_DEFINITION('material property','density of part',#27766);
#3955=AXIS2_PLACEMENT_3D('',#5130,#4288,#4289);
#3956=AXIS2_PLACEMENT_3D('',#5131,#4290,#4291);
#3957=AXIS2_PLACEMENT_3D('',#5194,#4294,#4295);
#3958=AXIS2_PLACEMENT_3D('',#5196,#4296,#4297);
#3959=AXIS2_PLACEMENT_3D('',#5198,#4298,#4299);
#3960=AXIS2_PLACEMENT_3D('',#5259,#4302,#4303);
#3961=AXIS2_PLACEMENT_3D('',#5260,#4304,#4305);
#3962=AXIS2_PLACEMENT_3D('',#5261,#4306,#4307);
#3963=AXIS2_PLACEMENT_3D('',#5262,#4308,#4309);
#3964=AXIS2_PLACEMENT_3D('',#5271,#4314,#4315);
#3965=AXIS2_PLACEMENT_3D('',#5277,#4319,#4320);
#3966=AXIS2_PLACEMENT_3D('',#5283,#4324,#4325);
#3967=AXIS2_PLACEMENT_3D('',#5289,#4329,#4330);
#3968=AXIS2_PLACEMENT_3D('',#5295,#4334,#4335);
#3969=AXIS2_PLACEMENT_3D('',#5298,#4338,#4339);
#3970=AXIS2_PLACEMENT_3D('',#5299,#4340,#4341);
#3971=AXIS2_PLACEMENT_3D('',#5300,#4342,#4343);
#3972=AXIS2_PLACEMENT_3D('',#5301,#4344,#4345);
#3973=AXIS2_PLACEMENT_3D('',#5379,#4347,#4348);
#3974=AXIS2_PLACEMENT_3D('',#5381,#4349,#4350);
#3975=AXIS2_PLACEMENT_3D('',#5384,#4352,#4353);
#3976=AXIS2_PLACEMENT_3D('',#5385,#4354,#4355);
#3977=AXIS2_PLACEMENT_3D('',#5387,#4356,#4357);
#3978=AXIS2_PLACEMENT_3D('',#5388,#4358,#4359);
#3979=AXIS2_PLACEMENT_3D('',#5390,#4360,#4361);
#3980=AXIS2_PLACEMENT_3D('',#5392,#4363,#4364);
#3981=AXIS2_PLACEMENT_3D('',#5394,#4365,#4366);
#3982=AXIS2_PLACEMENT_3D('',#5396,#4368,#4369);
#3983=AXIS2_PLACEMENT_3D('',#5399,#4371,#4372);
#3984=AXIS2_PLACEMENT_3D('',#5400,#4373,#4374);
#3985=AXIS2_PLACEMENT_3D('',#5402,#4375,#4376);
#3986=AXIS2_PLACEMENT_3D('',#5403,#4377,#4378);
#3987=AXIS2_PLACEMENT_3D('',#5405,#4379,#4380);
#3988=AXIS2_PLACEMENT_3D('',#5407,#4382,#4383);
#3989=AXIS2_PLACEMENT_3D('',#5409,#4384,#4385);
#3990=AXIS2_PLACEMENT_3D('',#5410,#4386,#4387);
#3991=AXIS2_PLACEMENT_3D('',#5412,#4388,#4389);
#3992=AXIS2_PLACEMENT_3D('',#5414,#4391,#4392);
#3993=AXIS2_PLACEMENT_3D('',#5415,#4393,#4394);
#3994=AXIS2_PLACEMENT_3D('',#5478,#4397,#4398);
#3995=AXIS2_PLACEMENT_3D('',#5480,#4399,#4400);
#3996=AXIS2_PLACEMENT_3D('',#5482,#4401,#4402);
#3997=AXIS2_PLACEMENT_3D('',#5543,#4405,#4406);
#3998=AXIS2_PLACEMENT_3D('',#5544,#4407,#4408);
#3999=AXIS2_PLACEMENT_3D('',#5545,#4409,#4410);
#4000=AXIS2_PLACEMENT_3D('',#5546,#4411,#4412);
#4001=AXIS2_PLACEMENT_3D('',#5555,#4417,#4418);
#4002=AXIS2_PLACEMENT_3D('',#5561,#4422,#4423);
#4003=AXIS2_PLACEMENT_3D('',#5567,#4427,#4428);
#4004=AXIS2_PLACEMENT_3D('',#5573,#4432,#4433);
#4005=AXIS2_PLACEMENT_3D('',#5579,#4437,#4438);
#4006=AXIS2_PLACEMENT_3D('',#5582,#4441,#4442);
#4007=AXIS2_PLACEMENT_3D('',#5583,#4443,#4444);
#4008=AXIS2_PLACEMENT_3D('',#5584,#4445,#4446);
#4009=AXIS2_PLACEMENT_3D('',#5585,#4447,#4448);
#4010=AXIS2_PLACEMENT_3D('',#5881,#4477,#4478);
#4011=AXIS2_PLACEMENT_3D('',#6177,#4507,#4508);
#4012=AXIS2_PLACEMENT_3D('',#6191,#4509,#4510);
#4013=AXIS2_PLACEMENT_3D('',#6192,#4511,#4512);
#4014=AXIS2_PLACEMENT_3D('',#6221,#4513,#4514);
#4015=AXIS2_PLACEMENT_3D('',#6250,#4515,#4516);
#4016=AXIS2_PLACEMENT_3D('',#6279,#4517,#4518);
#4017=AXIS2_PLACEMENT_3D('',#6308,#4519,#4520);
#4018=AXIS2_PLACEMENT_3D('',#6337,#4521,#4522);
#4019=AXIS2_PLACEMENT_3D('',#6366,#4523,#4524);
#4020=AXIS2_PLACEMENT_3D('',#6395,#4525,#4526);
#4021=AXIS2_PLACEMENT_3D('',#6424,#4527,#4528);
#4022=AXIS2_PLACEMENT_3D('',#6453,#4529,#4530);
#4023=AXIS2_PLACEMENT_3D('',#6482,#4531,#4532);
#4024=AXIS2_PLACEMENT_3D('',#6511,#4533,#4534);
#4025=AXIS2_PLACEMENT_3D('',#6540,#4535,#4536);
#4026=AXIS2_PLACEMENT_3D('',#6557,#4537,#4538);
#4027=AXIS2_PLACEMENT_3D('',#6585,#4539,#4540);
#4028=AXIS2_PLACEMENT_3D('',#6906,#4541,#4542);
#4029=AXIS2_PLACEMENT_3D('',#7087,#4543,#4544);
#4030=AXIS2_PLACEMENT_3D('',#7131,#4545,#4546);
#4031=AXIS2_PLACEMENT_3D('',#7132,#4547,#4548);
#4032=AXIS2_PLACEMENT_3D('',#7133,#4549,#4550);
#4033=AXIS2_PLACEMENT_3D('',#7141,#4551,#4552);
#4034=AXIS2_PLACEMENT_3D('',#7142,#4553,#4554);
#4035=AXIS2_PLACEMENT_3D('',#7204,#4555,#4556);
#4036=AXIS2_PLACEMENT_3D('',#7211,#4557,#4558);
#4037=AXIS2_PLACEMENT_3D('',#7218,#4559,#4560);
#4038=AXIS2_PLACEMENT_3D('',#7225,#4561,#4562);
#4039=AXIS2_PLACEMENT_3D('',#7232,#4563,#4564);
#4040=AXIS2_PLACEMENT_3D('',#7239,#4565,#4566);
#4041=AXIS2_PLACEMENT_3D('',#7246,#4567,#4568);
#4042=AXIS2_PLACEMENT_3D('',#7253,#4569,#4570);
#4043=AXIS2_PLACEMENT_3D('',#7260,#4571,#4572);
#4044=AXIS2_PLACEMENT_3D('',#7267,#4573,#4574);
#4045=AXIS2_PLACEMENT_3D('',#7274,#4575,#4576);
#4046=AXIS2_PLACEMENT_3D('',#7593,#4577,#4578);
#4047=AXIS2_PLACEMENT_3D('',#7616,#4579,#4580);
#4048=AXIS2_PLACEMENT_3D('',#7618,#4581,#4582);
#4049=AXIS2_PLACEMENT_3D('',#7621,#4584,#4585);
#4050=AXIS2_PLACEMENT_3D('',#7622,#4586,#4587);
#4051=AXIS2_PLACEMENT_3D('',#7623,#4588,#4589);
#4052=AXIS2_PLACEMENT_3D('',#7624,#4590,#4591);
#4053=AXIS2_PLACEMENT_3D('',#7625,#4592,#4593);
#4054=AXIS2_PLACEMENT_3D('',#7627,#4594,#4595);
#4055=AXIS2_PLACEMENT_3D('',#7629,#4596,#4597);
#4056=AXIS2_PLACEMENT_3D('',#7630,#4598,#4599);
#4057=AXIS2_PLACEMENT_3D('',#7631,#4600,#4601);
#4058=AXIS2_PLACEMENT_3D('',#7634,#4603,#4604);
#4059=AXIS2_PLACEMENT_3D('',#7635,#4605,#4606);
#4060=AXIS2_PLACEMENT_3D('',#7636,#4607,#4608);
#4061=AXIS2_PLACEMENT_3D('',#7638,#4609,#4610);
#4062=AXIS2_PLACEMENT_3D('',#7639,#4611,#4612);
#4063=AXIS2_PLACEMENT_3D('',#7640,#4613,#4614);
#4064=AXIS2_PLACEMENT_3D('',#7641,#4615,#4616);
#4065=AXIS2_PLACEMENT_3D('',#7642,#4617,#4618);
#4066=AXIS2_PLACEMENT_3D('',#7835,#4620,#4621);
#4067=AXIS2_PLACEMENT_3D('',#7972,#4622,#4623);
#4068=AXIS2_PLACEMENT_3D('',#8316,#4625,#4626);
#4069=AXIS2_PLACEMENT_3D('',#8650,#4628,#4629);
#4070=AXIS2_PLACEMENT_3D('',#8980,#4631,#4632);
#4071=AXIS2_PLACEMENT_3D('',#9316,#4634,#4635);
#4072=AXIS2_PLACEMENT_3D('',#9656,#4637,#4638);
#4073=AXIS2_PLACEMENT_3D('',#9873,#4639,#4640);
#4074=AXIS2_PLACEMENT_3D('',#10041,#4641,#4642);
#4075=AXIS2_PLACEMENT_3D('',#10163,#4643,#4644);
#4076=AXIS2_PLACEMENT_3D('',#12207,#4645,#4646);
#4077=AXIS2_PLACEMENT_3D('',#14502,#4647,#4648);
#4078=AXIS2_PLACEMENT_3D('',#14504,#4649,#4650);
#4079=AXIS2_PLACEMENT_3D('',#14514,#4651,#4652);
#4080=AXIS2_PLACEMENT_3D('',#14720,#4653,#4654);
#4081=AXIS2_PLACEMENT_3D('',#14722,#4655,#4656);
#4082=AXIS2_PLACEMENT_3D('',#14723,#4657,#4658);
#4083=AXIS2_PLACEMENT_3D('',#14724,#4659,#4660);
#4084=AXIS2_PLACEMENT_3D('',#14726,#4661,#4662);
#4085=AXIS2_PLACEMENT_3D('',#14728,#4664,#4665);
#4086=AXIS2_PLACEMENT_3D('',#15520,#4666,#4667);
#4087=AXIS2_PLACEMENT_3D('',#15522,#4668,#4669);
#4088=AXIS2_PLACEMENT_3D('',#15525,#4671,#4672);
#4089=AXIS2_PLACEMENT_3D('',#15526,#4673,#4674);
#4090=AXIS2_PLACEMENT_3D('',#15527,#4675,#4676);
#4091=AXIS2_PLACEMENT_3D('',#15528,#4677,#4678);
#4092=AXIS2_PLACEMENT_3D('',#15529,#4679,#4680);
#4093=AXIS2_PLACEMENT_3D('',#15530,#4681,#4682);
#4094=AXIS2_PLACEMENT_3D('',#15532,#4683,#4684);
#4095=AXIS2_PLACEMENT_3D('',#15535,#4686,#4687);
#4096=AXIS2_PLACEMENT_3D('',#15536,#4688,#4689);
#4097=AXIS2_PLACEMENT_3D('',#15538,#4690,#4691);
#4098=AXIS2_PLACEMENT_3D('',#15539,#4692,#4693);
#4099=AXIS2_PLACEMENT_3D('',#15542,#4695,#4696);
#4100=AXIS2_PLACEMENT_3D('',#15543,#4697,#4698);
#4101=AXIS2_PLACEMENT_3D('',#15621,#4700,#4701);
#4102=AXIS2_PLACEMENT_3D('',#15623,#4702,#4703);
#4103=AXIS2_PLACEMENT_3D('',#15626,#4705,#4706);
#4104=AXIS2_PLACEMENT_3D('',#15627,#4707,#4708);
#4105=AXIS2_PLACEMENT_3D('',#15629,#4709,#4710);
#4106=AXIS2_PLACEMENT_3D('',#15630,#4711,#4712);
#4107=AXIS2_PLACEMENT_3D('',#15632,#4713,#4714);
#4108=AXIS2_PLACEMENT_3D('',#15635,#4716,#4717);
#4109=AXIS2_PLACEMENT_3D('',#15636,#4718,#4719);
#4110=AXIS2_PLACEMENT_3D('',#15638,#4720,#4721);
#4111=AXIS2_PLACEMENT_3D('',#15640,#4723,#4724);
#4112=AXIS2_PLACEMENT_3D('',#15643,#4726,#4727);
#4113=AXIS2_PLACEMENT_3D('',#15644,#4728,#4729);
#4114=AXIS2_PLACEMENT_3D('',#15646,#4731,#4732);
#4115=AXIS2_PLACEMENT_3D('',#15648,#4733,#4734);
#4116=AXIS2_PLACEMENT_3D('',#15650,#4736,#4737);
#4117=AXIS2_PLACEMENT_3D('',#15652,#4738,#4739);
#4118=AXIS2_PLACEMENT_3D('',#15654,#4741,#4742);
#4119=AXIS2_PLACEMENT_3D('',#15656,#4743,#4744);
#4120=AXIS2_PLACEMENT_3D('',#15658,#4746,#4747);
#4121=AXIS2_PLACEMENT_3D('',#15660,#4748,#4749);
#4122=AXIS2_PLACEMENT_3D('',#15661,#4750,#4751);
#4123=AXIS2_PLACEMENT_3D('',#15663,#4752,#4753);
#4124=AXIS2_PLACEMENT_3D('',#15665,#4755,#4756);
#4125=AXIS2_PLACEMENT_3D('',#15667,#4757,#4758);
#4126=AXIS2_PLACEMENT_3D('',#15668,#4759,#4760);
#4127=AXIS2_PLACEMENT_3D('',#15670,#4761,#4762);
#4128=AXIS2_PLACEMENT_3D('',#15672,#4764,#4765);
#4129=AXIS2_PLACEMENT_3D('',#15674,#4766,#4767);
#4130=AXIS2_PLACEMENT_3D('',#15676,#4769,#4770);
#4131=AXIS2_PLACEMENT_3D('',#15678,#4771,#4772);
#4132=AXIS2_PLACEMENT_3D('',#15680,#4774,#4775);
#4133=AXIS2_PLACEMENT_3D('',#15682,#4776,#4777);
#4134=AXIS2_PLACEMENT_3D('',#15684,#4779,#4780);
#4135=AXIS2_PLACEMENT_3D('',#15686,#4781,#4782);
#4136=AXIS2_PLACEMENT_3D('',#15688,#4784,#4785);
#4137=AXIS2_PLACEMENT_3D('',#15690,#4786,#4787);
#4138=AXIS2_PLACEMENT_3D('',#15691,#4788,#4789);
#4139=AXIS2_PLACEMENT_3D('',#15693,#4790,#4791);
#4140=AXIS2_PLACEMENT_3D('',#15695,#4793,#4794);
#4141=AXIS2_PLACEMENT_3D('',#15697,#4795,#4796);
#4142=AXIS2_PLACEMENT_3D('',#15698,#4797,#4798);
#4143=AXIS2_PLACEMENT_3D('',#15700,#4800,#4801);
#4144=AXIS2_PLACEMENT_3D('',#15701,#4802,#4803);
#4145=AXIS2_PLACEMENT_3D('',#15702,#4804,#4805);
#4146=AXIS2_PLACEMENT_3D('',#15704,#4806,#4807);
#4147=AXIS2_PLACEMENT_3D('',#15706,#4808,#4809);
#4148=AXIS2_PLACEMENT_3D('',#15707,#4810,#4811);
#4149=AXIS2_PLACEMENT_3D('',#15708,#4812,#4813);
#4150=AXIS2_PLACEMENT_3D('',#15711,#4815,#4816);
#4151=AXIS2_PLACEMENT_3D('',#15712,#4817,#4818);
#4152=AXIS2_PLACEMENT_3D('',#15713,#4819,#4820);
#4153=AXIS2_PLACEMENT_3D('',#15715,#4821,#4822);
#4154=AXIS2_PLACEMENT_3D('',#15716,#4823,#4824);
#4155=AXIS2_PLACEMENT_3D('',#15717,#4825,#4826);
#4156=AXIS2_PLACEMENT_3D('',#15718,#4827,#4828);
#4157=AXIS2_PLACEMENT_3D('',#15719,#4829,#4830);
#4158=AXIS2_PLACEMENT_3D('',#15861,#4832,#4833);
#4159=AXIS2_PLACEMENT_3D('',#15864,#4835,#4836);
#4160=AXIS2_PLACEMENT_3D('',#15866,#4837,#4838);
#4161=AXIS2_PLACEMENT_3D('',#15975,#4839,#4840);
#4162=AXIS2_PLACEMENT_3D('',#16399,#4842,#4843);
#4163=AXIS2_PLACEMENT_3D('',#16799,#4845,#4846);
#4164=AXIS2_PLACEMENT_3D('',#17233,#4848,#4849);
#4165=AXIS2_PLACEMENT_3D('',#17645,#4851,#4852);
#4166=AXIS2_PLACEMENT_3D('',#18049,#4854,#4855);
#4167=AXIS2_PLACEMENT_3D('',#18467,#4857,#4858);
#4168=AXIS2_PLACEMENT_3D('',#18869,#4860,#4861);
#4169=AXIS2_PLACEMENT_3D('',#19293,#4863,#4864);
#4170=AXIS2_PLACEMENT_3D('',#19717,#4866,#4867);
#4171=AXIS2_PLACEMENT_3D('',#20143,#4869,#4870);
#4172=AXIS2_PLACEMENT_3D('',#20551,#4872,#4873);
#4173=AXIS2_PLACEMENT_3D('',#20957,#4875,#4876);
#4174=AXIS2_PLACEMENT_3D('',#21113,#4878,#4879);
#4175=AXIS2_PLACEMENT_3D('',#21256,#4880,#4881);
#4176=AXIS2_PLACEMENT_3D('',#21632,#4883,#4884);
#4177=AXIS2_PLACEMENT_3D('',#22033,#4886,#4887);
#4178=AXIS2_PLACEMENT_3D('',#22415,#4889,#4890);
#4179=AXIS2_PLACEMENT_3D('',#22801,#4892,#4893);
#4180=AXIS2_PLACEMENT_3D('',#23193,#4895,#4896);
#4181=AXIS2_PLACEMENT_3D('',#23575,#4898,#4899);
#4182=AXIS2_PLACEMENT_3D('',#23965,#4901,#4902);
#4183=AXIS2_PLACEMENT_3D('',#24343,#4904,#4905);
#4184=AXIS2_PLACEMENT_3D('',#24729,#4907,#4908);
#4185=AXIS2_PLACEMENT_3D('',#25113,#4910,#4911);
#4186=AXIS2_PLACEMENT_3D('',#25504,#4913,#4914);
#4187=AXIS2_PLACEMENT_3D('',#25892,#4916,#4917);
#4188=AXIS2_PLACEMENT_3D('',#26031,#4918,#4919);
#4189=AXIS2_PLACEMENT_3D('',#26139,#4920,#4921);
#4190=AXIS2_PLACEMENT_3D('',#26141,#4922,#4923);
#4191=AXIS2_PLACEMENT_3D('',#26143,#4925,#4926);
#4192=AXIS2_PLACEMENT_3D('',#26144,#4927,#4928);
#4193=AXIS2_PLACEMENT_3D('',#26328,#4929,#4930);
#4194=AXIS2_PLACEMENT_3D('',#26483,#4931,#4932);
#4195=AXIS2_PLACEMENT_3D('',#26485,#4933,#4934);
#4196=AXIS2_PLACEMENT_3D('',#26487,#4935,#4936);
#4197=AXIS2_PLACEMENT_3D('',#26488,#4937,#4938);
#4198=AXIS2_PLACEMENT_3D('',#26490,#4939,#4940);
#4199=AXIS2_PLACEMENT_3D('',#26492,#4941,#4942);
#4200=AXIS2_PLACEMENT_3D('',#26493,#4943,#4944);
#4201=AXIS2_PLACEMENT_3D('',#26494,#4945,#4946);
#4202=AXIS2_PLACEMENT_3D('',#26497,#4948,#4949);
#4203=AXIS2_PLACEMENT_3D('',#26498,#4950,#4951);
#4204=AXIS2_PLACEMENT_3D('',#26499,#4952,#4953);
#4205=AXIS2_PLACEMENT_3D('',#26500,#4954,#4955);
#4206=AXIS2_PLACEMENT_3D('',#26502,#4956,#4957);
#4207=AXIS2_PLACEMENT_3D('',#27028,#4958,#4959);
#4208=AXIS2_PLACEMENT_3D('',#27566,#4960,#4961);
#4209=AXIS2_PLACEMENT_3D('',#27567,#4962,#4963);
#4210=AXIS2_PLACEMENT_3D('',#27569,#4964,#4965);
#4211=AXIS2_PLACEMENT_3D('',#27571,#4966,#4967);
#4212=AXIS2_PLACEMENT_3D('',#27572,#4968,#4969);
#4213=AXIS2_PLACEMENT_3D('',#27573,#4970,#4971);
#4214=AXIS2_PLACEMENT_3D('',#27576,#4973,#4974);
#4215=AXIS2_PLACEMENT_3D('',#27577,#4975,#4976);
#4216=AXIS2_PLACEMENT_3D('',#27578,#4977,#4978);
#4217=AXIS2_PLACEMENT_3D('',#27580,#4979,#4980);
#4218=AXIS2_PLACEMENT_3D('',#27582,#4981,#4982);
#4219=AXIS2_PLACEMENT_3D('',#27583,#4983,#4984);
#4220=AXIS2_PLACEMENT_3D('',#27584,#4985,#4986);
#4221=AXIS2_PLACEMENT_3D('',#27587,#4988,#4989);
#4222=AXIS2_PLACEMENT_3D('',#27588,#4990,#4991);
#4223=AXIS2_PLACEMENT_3D('',#27589,#4992,#4993);
#4224=AXIS2_PLACEMENT_3D('',#27591,#4994,#4995);
#4225=AXIS2_PLACEMENT_3D('',#27592,#4996,#4997);
#4226=AXIS2_PLACEMENT_3D('',#27593,#4998,#4999);
#4227=AXIS2_PLACEMENT_3D('',#27595,#5000,#5001);
#4228=AXIS2_PLACEMENT_3D('',#27596,#5002,#5003);
#4229=AXIS2_PLACEMENT_3D('',#27598,#5004,#5005);
#4230=AXIS2_PLACEMENT_3D('',#27600,#5006,#5007);
#4231=AXIS2_PLACEMENT_3D('',#27601,#5008,#5009);
#4232=AXIS2_PLACEMENT_3D('',#27602,#5010,#5011);
#4233=AXIS2_PLACEMENT_3D('',#27605,#5013,#5014);
#4234=AXIS2_PLACEMENT_3D('',#27606,#5015,#5016);
#4235=AXIS2_PLACEMENT_3D('',#27608,#5017,#5018);
#4236=AXIS2_PLACEMENT_3D('',#27609,#5019,#5020);
#4237=AXIS2_PLACEMENT_3D('',#27610,#5021,#5022);
#4238=AXIS2_PLACEMENT_3D('',#27611,#5023,#5024);
#4239=AXIS2_PLACEMENT_3D('',#27613,#5025,#5026);
#4240=AXIS2_PLACEMENT_3D('',#27614,#5027,#5028);
#4241=AXIS2_PLACEMENT_3D('',#27615,#5029,#5030);
#4242=AXIS2_PLACEMENT_3D('',#27618,#5032,#5033);
#4243=AXIS2_PLACEMENT_3D('',#27619,#5034,#5035);
#4244=AXIS2_PLACEMENT_3D('',#27621,#5036,#5037);
#4245=AXIS2_PLACEMENT_3D('',#27622,#5038,#5039);
#4246=AXIS2_PLACEMENT_3D('',#27623,#5040,#5041);
#4247=AXIS2_PLACEMENT_3D('',#27625,#5042,#5043);
#4248=AXIS2_PLACEMENT_3D('',#27626,#5044,#5045);
#4249=AXIS2_PLACEMENT_3D('',#27628,#5046,#5047);
#4250=AXIS2_PLACEMENT_3D('',#27630,#5048,#5049);
#4251=AXIS2_PLACEMENT_3D('',#27631,#5050,#5051);
#4252=AXIS2_PLACEMENT_3D('',#27632,#5052,#5053);
#4253=AXIS2_PLACEMENT_3D('',#27635,#5055,#5056);
#4254=AXIS2_PLACEMENT_3D('',#27636,#5057,#5058);
#4255=AXIS2_PLACEMENT_3D('',#27638,#5059,#5060);
#4256=AXIS2_PLACEMENT_3D('',#27639,#5061,#5062);
#4257=AXIS2_PLACEMENT_3D('',#27641,#5063,#5064);
#4258=AXIS2_PLACEMENT_3D('',#27642,#5065,#5066);
#4259=AXIS2_PLACEMENT_3D('',#27643,#5067,#5068);
#4260=AXIS2_PLACEMENT_3D('',#27645,#5069,#5070);
#4261=AXIS2_PLACEMENT_3D('',#27646,#5071,#5072);
#4262=AXIS2_PLACEMENT_3D('',#27648,#5073,#5074);
#4263=AXIS2_PLACEMENT_3D('',#27650,#5075,#5076);
#4264=AXIS2_PLACEMENT_3D('',#27651,#5077,#5078);
#4265=AXIS2_PLACEMENT_3D('',#27652,#5079,#5080);
#4266=AXIS2_PLACEMENT_3D('',#27653,#5081,#5082);
#4267=AXIS2_PLACEMENT_3D('',#27655,#5084,#5085);
#4268=AXIS2_PLACEMENT_3D('',#27657,#5087,#5088);
#4269=AXIS2_PLACEMENT_3D('',#27659,#5090,#5091);
#4270=AXIS2_PLACEMENT_3D('',#27660,#5092,#5093);
#4271=AXIS2_PLACEMENT_3D('',#27662,#5094,#5095);
#4272=AXIS2_PLACEMENT_3D('',#27665,#5097,#5098);
#4273=AXIS2_PLACEMENT_3D('',#27666,#5099,#5100);
#4274=AXIS2_PLACEMENT_3D('',#27668,#5101,#5102);
#4275=AXIS2_PLACEMENT_3D('',#27669,#5103,#5104);
#4276=AXIS2_PLACEMENT_3D('',#27671,#5105,#5106);
#4277=AXIS2_PLACEMENT_3D('',#27673,#5108,#5109);
#4278=AXIS2_PLACEMENT_3D('',#27674,#5110,#5111);
#4279=AXIS2_PLACEMENT_3D('',#27675,#5112,#5113);
#4280=AXIS2_PLACEMENT_3D('',#27676,#5114,#5115);
#4281=AXIS2_PLACEMENT_3D('',#27677,#5116,#5117);
#4282=AXIS2_PLACEMENT_3D('',#27678,#5118,#5119);
#4283=AXIS2_PLACEMENT_3D('',#27679,#5120,#5121);
#4284=AXIS2_PLACEMENT_3D('',#27680,#5122,#5123);
#4285=AXIS2_PLACEMENT_3D('',#27681,#5124,#5125);
#4286=AXIS2_PLACEMENT_3D('',#27682,#5126,#5127);
#4287=AXIS2_PLACEMENT_3D('',#27683,#5128,#5129);
#4288=DIRECTION('axis',(0.,0.,1.));
#4289=DIRECTION('refdir',(1.,0.,0.));
#4290=DIRECTION('axis',(0.,0.,1.));
#4291=DIRECTION('refdir',(1.,0.,0.));
#4292=DIRECTION('',(1.,0.,0.));
#4293=DIRECTION('',(1.,0.,0.));
#4294=DIRECTION('center_axis',(1.,0.,0.));
#4295=DIRECTION('ref_axis',(0.,0.444750988585694,0.895654262621492));
#4296=DIRECTION('center_axis',(-1.,0.,0.));
#4297=DIRECTION('ref_axis',(0.,0.444750988585694,0.895654262621492));
#4298=DIRECTION('center_axis',(-1.,0.,0.));
#4299=DIRECTION('ref_axis',(0.,0.444750988585694,0.895654262621492));
#4300=DIRECTION('',(1.,0.,0.));
#4301=DIRECTION('',(1.,0.,0.));
#4302=DIRECTION('center_axis',(1.,0.,0.));
#4303=DIRECTION('ref_axis',(0.,-0.580623944517215,-0.814171870708679));
#4304=DIRECTION('center_axis',(-1.,0.,0.));
#4305=DIRECTION('ref_axis',(0.,-0.580623944517215,-0.814171870708679));
#4306=DIRECTION('center_axis',(-1.,0.,0.));
#4307=DIRECTION('ref_axis',(0.,-0.580623944517215,-0.814171870708679));
#4308=DIRECTION('center_axis',(0.,0.866025403784439,0.5));
#4309=DIRECTION('ref_axis',(0.,-0.5,0.866025403784439));
#4310=DIRECTION('',(0.,-0.5,0.866025403784439));
#4311=DIRECTION('',(1.,0.,0.));
#4312=DIRECTION('',(0.,-0.5,0.866025403784439));
#4313=DIRECTION('',(1.,0.,0.));
#4314=DIRECTION('center_axis',(0.,0.866025403784438,-0.5));
#4315=DIRECTION('ref_axis',(0.,0.5,0.866025403784438));
#4316=DIRECTION('',(0.,0.5,0.866025403784438));
#4317=DIRECTION('',(0.,0.5,0.866025403784438));
#4318=DIRECTION('',(1.,0.,0.));
#4319=DIRECTION('center_axis',(0.,-3.02823770847138E-16,-1.));
#4320=DIRECTION('ref_axis',(0.,1.,-3.02823770847138E-16));
#4321=DIRECTION('',(0.,1.,-3.02823770847138E-16));
#4322=DIRECTION('',(0.,1.,-3.02823770847138E-16));
#4323=DIRECTION('',(1.,0.,0.));
#4324=DIRECTION('center_axis',(0.,-0.866025403784439,-0.5));
#4325=DIRECTION('ref_axis',(0.,0.5,-0.866025403784439));
#4326=DIRECTION('',(0.,0.5,-0.866025403784439));
#4327=DIRECTION('',(0.,0.5,-0.866025403784439));
#4328=DIRECTION('',(1.,0.,0.));
#4329=DIRECTION('center_axis',(0.,-0.866025403784439,0.5));
#4330=DIRECTION('ref_axis',(0.,-0.5,-0.866025403784439));
#4331=DIRECTION('',(0.,-0.5,-0.866025403784439));
#4332=DIRECTION('',(0.,-0.5,-0.866025403784439));
#4333=DIRECTION('',(1.,0.,0.));
#4334=DIRECTION('center_axis',(0.,6.05647541694275E-16,1.));
#4335=DIRECTION('ref_axis',(0.,-1.,6.05647541694275E-16));
#4336=DIRECTION('',(0.,-1.,6.05647541694275E-16));
#4337=DIRECTION('',(0.,-1.,6.05647541694275E-16));
#4338=DIRECTION('center_axis',(1.,0.,0.));
#4339=DIRECTION('ref_axis',(0.,1.,0.));
#4340=DIRECTION('center_axis',(1.,0.,0.));
#4341=DIRECTION('ref_axis',(0.,1.,0.));
#4342=DIRECTION('axis',(0.,0.,1.));
#4343=DIRECTION('refdir',(1.,0.,0.));
#4344=DIRECTION('center_axis',(0.,1.,0.));
#4345=DIRECTION('ref_axis',(1.,0.,0.));
#4346=DIRECTION('',(0.,1.,0.));
#4347=DIRECTION('center_axis',(1.,0.,0.));
#4348=DIRECTION('ref_axis',(0.,1.,0.));
#4349=DIRECTION('center_axis',(1.,0.,0.));
#4350=DIRECTION('ref_axis',(0.,0.,-1.));
#4351=DIRECTION('',(1.,0.,0.));
#4352=DIRECTION('center_axis',(1.,0.,0.));
#4353=DIRECTION('ref_axis',(0.,0.,-1.));
#4354=DIRECTION('center_axis',(-1.,0.,0.));
#4355=DIRECTION('ref_axis',(0.,0.,1.));
#4356=DIRECTION('center_axis',(1.,0.,0.));
#4357=DIRECTION('ref_axis',(0.,0.,-1.));
#4358=DIRECTION('center_axis',(1.,0.,0.));
#4359=DIRECTION('ref_axis',(0.,1.,0.));
#4360=DIRECTION('center_axis',(1.,0.,0.));
#4361=DIRECTION('ref_axis',(0.,0.,-1.));
#4362=DIRECTION('',(-0.777301434879696,0.629128348855753,7.70460018679057E-17));
#4363=DIRECTION('center_axis',(1.,0.,0.));
#4364=DIRECTION('ref_axis',(0.,1.,0.));
#4365=DIRECTION('center_axis',(1.,0.,0.));
#4366=DIRECTION('ref_axis',(0.,0.,-1.));
#4367=DIRECTION('',(-1.,0.,0.));
#4368=DIRECTION('center_axis',(-1.,0.,0.));
#4369=DIRECTION('ref_axis',(0.,1.,0.));
#4370=DIRECTION('',(0.687853663884889,0.725849390080431,-8.88909132225059E-17));
#4371=DIRECTION('center_axis',(1.,0.,0.));
#4372=DIRECTION('ref_axis',(0.,0.,-1.));
#4373=DIRECTION('center_axis',(1.,0.,0.));
#4374=DIRECTION('ref_axis',(0.,0.,-1.));
#4375=DIRECTION('center_axis',(1.,0.,0.));
#4376=DIRECTION('ref_axis',(0.,0.,-1.));
#4377=DIRECTION('center_axis',(1.,0.,0.));
#4378=DIRECTION('ref_axis',(0.,1.,0.));
#4379=DIRECTION('center_axis',(1.,0.,0.));
#4380=DIRECTION('ref_axis',(0.,0.,-1.));
#4381=DIRECTION('',(1.,0.,0.));
#4382=DIRECTION('center_axis',(1.,0.,0.));
#4383=DIRECTION('ref_axis',(0.,0.,-1.));
#4384=DIRECTION('center_axis',(1.,0.,0.));
#4385=DIRECTION('ref_axis',(0.,0.,-1.));
#4386=DIRECTION('center_axis',(1.,0.,0.));
#4387=DIRECTION('ref_axis',(0.,1.,0.));
#4388=DIRECTION('center_axis',(1.,0.,0.));
#4389=DIRECTION('ref_axis',(0.,0.,-1.));
#4390=DIRECTION('',(1.,0.,0.));
#4391=DIRECTION('center_axis',(-1.,0.,0.));
#4392=DIRECTION('ref_axis',(0.,0.,1.));
#4393=DIRECTION('axis',(0.,0.,1.));
#4394=DIRECTION('refdir',(1.,0.,0.));
#4395=DIRECTION('',(1.,0.,0.));
#4396=DIRECTION('',(1.,0.,0.));
#4397=DIRECTION('center_axis',(1.,0.,0.));
#4398=DIRECTION('ref_axis',(0.,0.444750988585694,0.895654262621492));
#4399=DIRECTION('center_axis',(-1.,0.,0.));
#4400=DIRECTION('ref_axis',(0.,0.444750988585694,0.895654262621492));
#4401=DIRECTION('center_axis',(-1.,0.,0.));
#4402=DIRECTION('ref_axis',(0.,0.444750988585694,0.895654262621492));
#4403=DIRECTION('',(1.,0.,0.));
#4404=DIRECTION('',(1.,0.,0.));
#4405=DIRECTION('center_axis',(1.,0.,0.));
#4406=DIRECTION('ref_axis',(0.,-0.580623944517215,-0.814171870708679));
#4407=DIRECTION('center_axis',(-1.,0.,0.));
#4408=DIRECTION('ref_axis',(0.,-0.580623944517215,-0.814171870708679));
#4409=DIRECTION('center_axis',(-1.,0.,0.));
#4410=DIRECTION('ref_axis',(0.,-0.580623944517215,-0.814171870708679));
#4411=DIRECTION('center_axis',(0.,0.866025403784439,0.5));
#4412=DIRECTION('ref_axis',(0.,-0.5,0.866025403784439));
#4413=DIRECTION('',(0.,-0.5,0.866025403784439));
#4414=DIRECTION('',(1.,0.,0.));
#4415=DIRECTION('',(0.,-0.5,0.866025403784439));
#4416=DIRECTION('',(1.,0.,0.));
#4417=DIRECTION('center_axis',(0.,0.866025403784438,-0.5));
#4418=DIRECTION('ref_axis',(0.,0.5,0.866025403784438));
#4419=DIRECTION('',(0.,0.5,0.866025403784438));
#4420=DIRECTION('',(0.,0.5,0.866025403784438));
#4421=DIRECTION('',(1.,0.,0.));
#4422=DIRECTION('center_axis',(0.,-3.02823770847138E-16,-1.));
#4423=DIRECTION('ref_axis',(0.,1.,-3.02823770847138E-16));
#4424=DIRECTION('',(0.,1.,-3.02823770847138E-16));
#4425=DIRECTION('',(0.,1.,-3.02823770847138E-16));
#4426=DIRECTION('',(1.,0.,0.));
#4427=DIRECTION('center_axis',(0.,-0.866025403784439,-0.5));
#4428=DIRECTION('ref_axis',(0.,0.5,-0.866025403784439));
#4429=DIRECTION('',(0.,0.5,-0.866025403784439));
#4430=DIRECTION('',(0.,0.5,-0.866025403784439));
#4431=DIRECTION('',(1.,0.,0.));
#4432=DIRECTION('center_axis',(0.,-0.866025403784439,0.5));
#4433=DIRECTION('ref_axis',(0.,-0.5,-0.866025403784439));
#4434=DIRECTION('',(0.,-0.5,-0.866025403784439));
#4435=DIRECTION('',(0.,-0.5,-0.866025403784439));
#4436=DIRECTION('',(1.,0.,0.));
#4437=DIRECTION('center_axis',(0.,6.05647541694275E-16,1.));
#4438=DIRECTION('ref_axis',(0.,-1.,6.05647541694275E-16));
#4439=DIRECTION('',(0.,-1.,6.05647541694275E-16));
#4440=DIRECTION('',(0.,-1.,6.05647541694275E-16));
#4441=DIRECTION('center_axis',(1.,0.,0.));
#4442=DIRECTION('ref_axis',(0.,1.,0.));
#4443=DIRECTION('center_axis',(1.,0.,0.));
#4444=DIRECTION('ref_axis',(0.,1.,0.));
#4445=DIRECTION('axis',(0.,0.,1.));
#4446=DIRECTION('refdir',(1.,0.,0.));
#4447=DIRECTION('center_axis',(0.,1.,0.));
#4448=DIRECTION('ref_axis',(0.,0.,1.));
#4449=DIRECTION('',(0.,0.,1.));
#4450=DIRECTION('',(1.,0.,0.));
#4451=DIRECTION('',(1.,0.,0.));
#4452=DIRECTION('',(1.,0.,0.));
#4453=DIRECTION('',(1.,0.,0.));
#4454=DIRECTION('',(1.,0.,0.));
#4455=DIRECTION('',(1.,0.,0.));
#4456=DIRECTION('',(1.,0.,0.));
#4457=DIRECTION('',(1.,0.,0.));
#4458=DIRECTION('',(1.,0.,0.));
#4459=DIRECTION('',(1.,0.,0.));
#4460=DIRECTION('',(1.,0.,0.));
#4461=DIRECTION('',(1.,0.,0.));
#4462=DIRECTION('',(1.,0.,0.));
#4463=DIRECTION('',(0.,0.,1.));
#4464=DIRECTION('',(-1.,0.,0.));
#4465=DIRECTION('',(-1.,0.,0.));
#4466=DIRECTION('',(-1.,0.,0.));
#4467=DIRECTION('',(-1.,0.,0.));
#4468=DIRECTION('',(-1.,0.,0.));
#4469=DIRECTION('',(-1.,0.,0.));
#4470=DIRECTION('',(-1.,0.,0.));
#4471=DIRECTION('',(-1.,0.,0.));
#4472=DIRECTION('',(-1.,0.,0.));
#4473=DIRECTION('',(-1.,0.,0.));
#4474=DIRECTION('',(-1.,0.,0.));
#4475=DIRECTION('',(-1.,0.,0.));
#4476=DIRECTION('',(-1.,0.,0.));
#4477=DIRECTION('center_axis',(0.,-1.,0.));
#4478=DIRECTION('ref_axis',(0.,0.,-1.));
#4479=DIRECTION('',(1.,0.,0.));
#4480=DIRECTION('',(1.,0.,0.));
#4481=DIRECTION('',(1.,0.,0.));
#4482=DIRECTION('',(1.,0.,0.));
#4483=DIRECTION('',(1.,0.,0.));
#4484=DIRECTION('',(1.,0.,0.));
#4485=DIRECTION('',(1.,0.,0.));
#4486=DIRECTION('',(1.,0.,0.));
#4487=DIRECTION('',(1.,0.,0.));
#4488=DIRECTION('',(1.,0.,0.));
#4489=DIRECTION('',(1.,0.,0.));
#4490=DIRECTION('',(1.,0.,0.));
#4491=DIRECTION('',(1.,0.,0.));
#4492=DIRECTION('',(0.,0.,-1.));
#4493=DIRECTION('',(-1.,0.,0.));
#4494=DIRECTION('',(-1.,0.,0.));
#4495=DIRECTION('',(-1.,0.,0.));
#4496=DIRECTION('',(-1.,0.,0.));
#4497=DIRECTION('',(-1.,0.,0.));
#4498=DIRECTION('',(-1.,0.,0.));
#4499=DIRECTION('',(-1.,0.,0.));
#4500=DIRECTION('',(-1.,0.,0.));
#4501=DIRECTION('',(-1.,0.,0.));
#4502=DIRECTION('',(-1.,0.,0.));
#4503=DIRECTION('',(-1.,0.,0.));
#4504=DIRECTION('',(-1.,0.,0.));
#4505=DIRECTION('',(-1.,0.,0.));
#4506=DIRECTION('',(0.,0.,-1.));
#4507=DIRECTION('center_axis',(-1.,0.,0.));
#4508=DIRECTION('ref_axis',(0.,-1.,2.19773242311135E-14));
#4509=DIRECTION('center_axis',(-1.,0.,0.));
#4510=DIRECTION('ref_axis',(0.,-1.,2.19773242311135E-14));
#4511=DIRECTION('center_axis',(-1.,0.,0.));
#4512=DIRECTION('ref_axis',(0.,-1.,2.19773242311135E-14));
#4513=DIRECTION('center_axis',(-1.,0.,0.));
#4514=DIRECTION('ref_axis',(0.,-1.,2.19773242311135E-14));
#4515=DIRECTION('center_axis',(-1.,0.,0.));
#4516=DIRECTION('ref_axis',(0.,-1.,2.19773242311135E-14));
#4517=DIRECTION('center_axis',(-1.,0.,0.));
#4518=DIRECTION('ref_axis',(0.,-1.,2.19773242311135E-14));
#4519=DIRECTION('center_axis',(-1.,0.,0.));
#4520=DIRECTION('ref_axis',(0.,-1.,2.19773242311135E-14));
#4521=DIRECTION('center_axis',(-1.,0.,0.));
#4522=DIRECTION('ref_axis',(0.,-1.,2.19773242311135E-14));
#4523=DIRECTION('center_axis',(-1.,0.,0.));
#4524=DIRECTION('ref_axis',(0.,-1.,2.19773242311135E-14));
#4525=DIRECTION('center_axis',(-1.,0.,0.));
#4526=DIRECTION('ref_axis',(0.,-1.,2.19773242311135E-14));
#4527=DIRECTION('center_axis',(-1.,0.,0.));
#4528=DIRECTION('ref_axis',(0.,-1.,2.19773242311135E-14));
#4529=DIRECTION('center_axis',(-1.,0.,0.));
#4530=DIRECTION('ref_axis',(0.,-1.,2.19773242311135E-14));
#4531=DIRECTION('center_axis',(-1.,0.,0.));
#4532=DIRECTION('ref_axis',(0.,-1.,2.19773242311135E-14));
#4533=DIRECTION('center_axis',(-1.,0.,0.));
#4534=DIRECTION('ref_axis',(0.,-1.,2.19773242311135E-14));
#4535=DIRECTION('center_axis',(-1.,0.,0.));
#4536=DIRECTION('ref_axis',(0.,-1.,2.19773242311135E-14));
#4537=DIRECTION('center_axis',(1.,0.,0.));
#4538=DIRECTION('ref_axis',(0.,-1.,2.19773242311135E-14));
#4539=DIRECTION('center_axis',(1.,2.26944640896891E-13,2.4756931710509E-13));
#4540=DIRECTION('ref_axis',(-2.99635666187292E-14,0.794492776111595,-0.607273602840179));
#4541=DIRECTION('center_axis',(1.,-4.24721344664965E-14,7.81460509822211E-14));
#4542=DIRECTION('ref_axis',(-1.5231504897179E-14,0.783860772073074,0.620936623179052));
#4543=DIRECTION('center_axis',(-1.,0.,0.));
#4544=DIRECTION('ref_axis',(0.,-1.,0.));
#4545=DIRECTION('center_axis',(1.,0.,0.));
#4546=DIRECTION('ref_axis',(0.,-1.,0.));
#4547=DIRECTION('center_axis',(-1.,0.,0.));
#4548=DIRECTION('ref_axis',(0.,-1.,0.));
#4549=DIRECTION('center_axis',(-1.,0.,0.));
#4550=DIRECTION('ref_axis',(0.,-1.,0.));
#4551=DIRECTION('center_axis',(1.,0.,0.));
#4552=DIRECTION('ref_axis',(0.,-1.,0.));
#4553=DIRECTION('center_axis',(-1.,0.,0.));
#4554=DIRECTION('ref_axis',(0.,-1.,0.));
#4555=DIRECTION('center_axis',(-1.,0.,0.));
#4556=DIRECTION('ref_axis',(0.,-1.,0.));
#4557=DIRECTION('center_axis',(-1.,0.,0.));
#4558=DIRECTION('ref_axis',(0.,-1.,0.));
#4559=DIRECTION('center_axis',(-1.,0.,0.));
#4560=DIRECTION('ref_axis',(0.,-1.,0.));
#4561=DIRECTION('center_axis',(-1.,0.,0.));
#4562=DIRECTION('ref_axis',(0.,-1.,0.));
#4563=DIRECTION('center_axis',(-1.,0.,0.));
#4564=DIRECTION('ref_axis',(0.,-1.,0.));
#4565=DIRECTION('center_axis',(-1.,0.,0.));
#4566=DIRECTION('ref_axis',(0.,-1.,0.));
#4567=DIRECTION('center_axis',(-1.,0.,0.));
#4568=DIRECTION('ref_axis',(0.,-1.,0.));
#4569=DIRECTION('center_axis',(-1.,0.,0.));
#4570=DIRECTION('ref_axis',(0.,-1.,0.));
#4571=DIRECTION('center_axis',(-1.,0.,0.));
#4572=DIRECTION('ref_axis',(0.,-1.,0.));
#4573=DIRECTION('center_axis',(-1.,0.,0.));
#4574=DIRECTION('ref_axis',(0.,-1.,0.));
#4575=DIRECTION('center_axis',(-1.,0.,0.));
#4576=DIRECTION('ref_axis',(0.,-1.,0.));
#4577=DIRECTION('center_axis',(1.,-7.18663344203148E-15,1.44094323913819E-14));
#4578=DIRECTION('ref_axis',(-4.36221174028662E-15,0.74050159851997,0.672054597922944));
#4579=DIRECTION('center_axis',(1.,0.,0.));
#4580=DIRECTION('ref_axis',(0.,-1.,0.));
#4581=DIRECTION('center_axis',(1.,0.,0.));
#4582=DIRECTION('ref_axis',(0.,-1.,0.));
#4583=DIRECTION('',(-1.,0.,0.));
#4584=DIRECTION('center_axis',(-1.,0.,0.));
#4585=DIRECTION('ref_axis',(0.,-1.,0.));
#4586=DIRECTION('center_axis',(-1.,0.,0.));
#4587=DIRECTION('ref_axis',(0.,-1.,0.));
#4588=DIRECTION('center_axis',(-1.,0.,0.));
#4589=DIRECTION('ref_axis',(0.,-1.,0.));
#4590=DIRECTION('axis',(0.,0.,1.));
#4591=DIRECTION('refdir',(1.,0.,0.));
#4592=DIRECTION('center_axis',(1.,0.,0.));
#4593=DIRECTION('ref_axis',(0.,0.,-1.));
#4594=DIRECTION('center_axis',(-1.,0.,0.));
#4595=DIRECTION('ref_axis',(0.,1.22464679914735E-16,1.));
#4596=DIRECTION('center_axis',(0.,-1.,-1.22464679914735E-16));
#4597=DIRECTION('ref_axis',(0.,-1.22464679914735E-16,1.));
#4598=DIRECTION('center_axis',(1.,0.,0.));
#4599=DIRECTION('ref_axis',(0.,0.,1.));
#4600=DIRECTION('center_axis',(1.,0.,0.));
#4601=DIRECTION('ref_axis',(0.,0.,-1.));
#4602=DIRECTION('',(-0.999999956307574,3.62016965808782E-20,-0.000295609285927038));
#4603=DIRECTION('center_axis',(-1.,0.,0.));
#4604=DIRECTION('ref_axis',(0.,0.,1.));
#4605=DIRECTION('center_axis',(1.,0.,0.));
#4606=DIRECTION('ref_axis',(0.,0.,-1.));
#4607=DIRECTION('center_axis',(1.,0.,0.));
#4608=DIRECTION('ref_axis',(0.,0.,-1.));
#4609=DIRECTION('center_axis',(0.,-1.,-1.22464679914735E-16));
#4610=DIRECTION('ref_axis',(0.,-1.22464679914735E-16,1.));
#4611=DIRECTION('center_axis',(1.,0.,0.));
#4612=DIRECTION('ref_axis',(0.,1.22464679914735E-16,1.));
#4613=DIRECTION('center_axis',(-1.,0.,0.));
#4614=DIRECTION('ref_axis',(0.,0.,1.));
#4615=DIRECTION('axis',(0.,0.,1.));
#4616=DIRECTION('refdir',(1.,0.,0.));
#4617=DIRECTION('center_axis',(1.,0.,0.));
#4618=DIRECTION('ref_axis',(0.,0.704081661975572,-0.710119013454587));
#4619=DIRECTION('',(-1.,0.,0.));
#4620=DIRECTION('center_axis',(-1.,0.,0.));
#4621=DIRECTION('ref_axis',(0.,1.,2.1444273868172E-14));
#4622=DIRECTION('center_axis',(1.,0.,0.));
#4623=DIRECTION('ref_axis',(0.,0.704081661975572,-0.710119013454587));
#4624=DIRECTION('',(-1.,0.,0.));
#4625=DIRECTION('center_axis',(1.,0.,0.));
#4626=DIRECTION('ref_axis',(0.,0.704081661975572,-0.710119013454587));
#4627=DIRECTION('',(-1.,0.,0.));
#4628=DIRECTION('center_axis',(1.,0.,0.));
#4629=DIRECTION('ref_axis',(0.,0.704081661975572,-0.710119013454587));
#4630=DIRECTION('',(-1.,0.,0.));
#4631=DIRECTION('center_axis',(1.,0.,0.));
#4632=DIRECTION('ref_axis',(0.,0.704081661975572,-0.710119013454587));
#4633=DIRECTION('',(-1.,0.,0.));
#4634=DIRECTION('center_axis',(1.,0.,0.));
#4635=DIRECTION('ref_axis',(0.,0.704081661975572,-0.710119013454587));
#4636=DIRECTION('',(-1.,0.,0.));
#4637=DIRECTION('center_axis',(1.,0.,0.));
#4638=DIRECTION('ref_axis',(0.,0.704081661975572,-0.710119013454587));
#4639=DIRECTION('center_axis',(1.,0.,0.));
#4640=DIRECTION('ref_axis',(0.,1.,2.1444273868172E-14));
#4641=DIRECTION('center_axis',(1.,0.,0.));
#4642=DIRECTION('ref_axis',(0.,1.,0.));
#4643=DIRECTION('center_axis',(-1.,0.,0.));
#4644=DIRECTION('ref_axis',(0.,1.,0.));
#4645=DIRECTION('center_axis',(-1.,0.,0.));
#4646=DIRECTION('ref_axis',(0.,1.,0.));
#4647=DIRECTION('center_axis',(1.,0.,0.));
#4648=DIRECTION('ref_axis',(0.,-0.692346234554118,0.72156544505591));
#4649=DIRECTION('center_axis',(-1.,0.,0.));
#4650=DIRECTION('ref_axis',(0.,9.28774802075533E-14,-1.));
#4651=DIRECTION('center_axis',(-1.,0.,0.));
#4652=DIRECTION('ref_axis',(0.,9.28774802075533E-14,-1.));
#4653=DIRECTION('center_axis',(1.,0.,0.));
#4654=DIRECTION('ref_axis',(0.,0.,-1.));
#4655=DIRECTION('center_axis',(-1.,0.,0.));
#4656=DIRECTION('ref_axis',(0.,0.,-1.));
#4657=DIRECTION('center_axis',(-1.,0.,0.));
#4658=DIRECTION('ref_axis',(0.,0.,-1.));
#4659=DIRECTION('center_axis',(1.,0.,0.));
#4660=DIRECTION('ref_axis',(0.,0.,-1.));
#4661=DIRECTION('center_axis',(1.,0.,0.));
#4662=DIRECTION('ref_axis',(0.,0.,-1.));
#4663=DIRECTION('',(1.,0.,0.));
#4664=DIRECTION('center_axis',(-1.,0.,0.));
#4665=DIRECTION('ref_axis',(0.,0.,-1.));
#4666=DIRECTION('center_axis',(1.,0.,0.));
#4667=DIRECTION('ref_axis',(0.,1.,0.));
#4668=DIRECTION('center_axis',(1.,0.,0.));
#4669=DIRECTION('ref_axis',(0.,1.,0.));
#4670=DIRECTION('',(-1.,0.,0.));
#4671=DIRECTION('center_axis',(1.,0.,0.));
#4672=DIRECTION('ref_axis',(0.,1.,0.));
#4673=DIRECTION('center_axis',(1.,0.,0.));
#4674=DIRECTION('ref_axis',(0.,1.,0.));
#4675=DIRECTION('center_axis',(1.,0.,0.));
#4676=DIRECTION('ref_axis',(0.,1.,0.));
#4677=DIRECTION('center_axis',(1.,0.,0.));
#4678=DIRECTION('ref_axis',(0.,1.,0.));
#4679=DIRECTION('axis',(0.,0.,1.));
#4680=DIRECTION('refdir',(1.,0.,0.));
#4681=DIRECTION('center_axis',(-1.,0.,0.));
#4682=DIRECTION('ref_axis',(0.,0.,-1.));
#4683=DIRECTION('center_axis',(1.,0.,0.));
#4684=DIRECTION('ref_axis',(0.,0.,-1.));
#4685=DIRECTION('',(0.707106781186546,-8.65956056235496E-17,-0.707106781186549));
#4686=DIRECTION('center_axis',(-1.,0.,0.));
#4687=DIRECTION('ref_axis',(0.,0.,-1.));
#4688=DIRECTION('center_axis',(-1.,0.,0.));
#4689=DIRECTION('ref_axis',(0.,0.,1.));
#4690=DIRECTION('center_axis',(1.,0.,0.));
#4691=DIRECTION('ref_axis',(0.,0.,-1.));
#4692=DIRECTION('center_axis',(1.,0.,0.));
#4693=DIRECTION('ref_axis',(0.,0.,-1.));
#4694=DIRECTION('',(-1.,0.,0.));
#4695=DIRECTION('center_axis',(1.,0.,0.));
#4696=DIRECTION('ref_axis',(0.,0.,-1.));
#4697=DIRECTION('center_axis',(0.,1.,0.));
#4698=DIRECTION('ref_axis',(1.,0.,0.));
#4699=DIRECTION('',(0.,1.,0.));
#4700=DIRECTION('center_axis',(1.,0.,0.));
#4701=DIRECTION('ref_axis',(0.,-1.,0.));
#4702=DIRECTION('center_axis',(1.,0.,0.));
#4703=DIRECTION('ref_axis',(0.,-1.,0.));
#4704=DIRECTION('',(1.,0.,0.));
#4705=DIRECTION('center_axis',(1.,0.,0.));
#4706=DIRECTION('ref_axis',(0.,-1.,0.));
#4707=DIRECTION('center_axis',(-1.,0.,0.));
#4708=DIRECTION('ref_axis',(0.,-1.,0.));
#4709=DIRECTION('center_axis',(1.,0.,0.));
#4710=DIRECTION('ref_axis',(0.,0.,-1.));
#4711=DIRECTION('center_axis',(1.,0.,0.));
#4712=DIRECTION('ref_axis',(0.,0.,-1.));
#4713=DIRECTION('center_axis',(1.,0.,0.));
#4714=DIRECTION('ref_axis',(0.,0.,-1.));
#4715=DIRECTION('',(-0.819194986126072,7.02353436578877E-17,-0.573515104165448));
#4716=DIRECTION('center_axis',(1.,0.,0.));
#4717=DIRECTION('ref_axis',(0.,0.,-1.));
#4718=DIRECTION('center_axis',(1.,0.,0.));
#4719=DIRECTION('ref_axis',(0.,0.,-1.));
#4720=DIRECTION('center_axis',(1.,0.,0.));
#4721=DIRECTION('ref_axis',(0.,0.,-1.));
#4722=DIRECTION('',(-1.,0.,0.));
#4723=DIRECTION('center_axis',(-1.,0.,0.));
#4724=DIRECTION('ref_axis',(0.,0.,-1.));
#4725=DIRECTION('',(0.848733460294827,-6.47618786727041E-17,-0.528820870783264));
#4726=DIRECTION('center_axis',(1.,0.,0.));
#4727=DIRECTION('ref_axis',(0.,0.,-1.));
#4728=DIRECTION('center_axis',(1.,0.,0.));
#4729=DIRECTION('ref_axis',(0.,0.,-1.));
#4730=DIRECTION('',(-0.819194986126072,7.02353436578877E-17,-0.573515104165448));
#4731=DIRECTION('center_axis',(1.,0.,0.));
#4732=DIRECTION('ref_axis',(0.,0.,-1.));
#4733=DIRECTION('center_axis',(1.,0.,0.));
#4734=DIRECTION('ref_axis',(0.,0.,-1.));
#4735=DIRECTION('',(0.999999956307574,-3.62016965809164E-20,0.00029560928592735));
#4736=DIRECTION('center_axis',(1.,0.,0.));
#4737=DIRECTION('ref_axis',(0.,0.,-1.));
#4738=DIRECTION('center_axis',(1.,0.,0.));
#4739=DIRECTION('ref_axis',(0.,0.,-1.));
#4740=DIRECTION('',(1.,0.,0.));
#4741=DIRECTION('center_axis',(1.,0.,0.));
#4742=DIRECTION('ref_axis',(0.,0.,-1.));
#4743=DIRECTION('center_axis',(1.,0.,0.));
#4744=DIRECTION('ref_axis',(0.,0.,-1.));
#4745=DIRECTION('',(0.999999956307574,-3.62016965809512E-20,0.000295609285927634));
#4746=DIRECTION('center_axis',(-1.,0.,0.));
#4747=DIRECTION('ref_axis',(0.,0.,1.));
#4748=DIRECTION('center_axis',(1.,0.,0.));
#4749=DIRECTION('ref_axis',(0.,0.,-1.));
#4750=DIRECTION('center_axis',(1.,0.,0.));
#4751=DIRECTION('ref_axis',(0.,0.,-1.));
#4752=DIRECTION('center_axis',(1.,0.,0.));
#4753=DIRECTION('ref_axis',(0.,0.,-1.));
#4754=DIRECTION('',(1.,0.,0.));
#4755=DIRECTION('center_axis',(1.,0.,0.));
#4756=DIRECTION('ref_axis',(0.,0.,-1.));
#4757=DIRECTION('center_axis',(1.,0.,0.));
#4758=DIRECTION('ref_axis',(0.,0.,-1.));
#4759=DIRECTION('center_axis',(1.,0.,0.));
#4760=DIRECTION('ref_axis',(0.,0.,-1.));
#4761=DIRECTION('center_axis',(1.,0.,0.));
#4762=DIRECTION('ref_axis',(0.,0.,-1.));
#4763=DIRECTION('',(0.999999956307574,-3.62016965809699E-20,0.000295609285927787));
#4764=DIRECTION('center_axis',(1.,0.,0.));
#4765=DIRECTION('ref_axis',(0.,0.,-1.));
#4766=DIRECTION('center_axis',(1.,0.,0.));
#4767=DIRECTION('ref_axis',(0.,0.,-1.));
#4768=DIRECTION('',(1.,0.,0.));
#4769=DIRECTION('center_axis',(1.,0.,0.));
#4770=DIRECTION('ref_axis',(0.,0.,-1.));
#4771=DIRECTION('center_axis',(1.,0.,0.));
#4772=DIRECTION('ref_axis',(0.,0.,-1.));
#4773=DIRECTION('',(0.999999956307574,-3.62016965808782E-20,0.000295609285927038));
#4774=DIRECTION('center_axis',(1.,0.,0.));
#4775=DIRECTION('ref_axis',(0.,0.,-1.));
#4776=DIRECTION('center_axis',(1.,0.,0.));
#4777=DIRECTION('ref_axis',(0.,0.,-1.));
#4778=DIRECTION('',(1.,0.,0.));
#4779=DIRECTION('center_axis',(1.,0.,0.));
#4780=DIRECTION('ref_axis',(0.,0.,-1.));
#4781=DIRECTION('center_axis',(1.,0.,0.));
#4782=DIRECTION('ref_axis',(0.,0.,-1.));
#4783=DIRECTION('',(0.999999956307574,-3.62016965808193E-20,0.000295609285926557));
#4784=DIRECTION('center_axis',(1.,0.,0.));
#4785=DIRECTION('ref_axis',(0.,0.,-1.));
#4786=DIRECTION('center_axis',(1.,0.,0.));
#4787=DIRECTION('ref_axis',(0.,0.,-1.));
#4788=DIRECTION('center_axis',(1.,0.,0.));
#4789=DIRECTION('ref_axis',(0.,0.,-1.));
#4790=DIRECTION('center_axis',(1.,0.,0.));
#4791=DIRECTION('ref_axis',(0.,0.,-1.));
#4792=DIRECTION('',(1.,0.,0.));
#4793=DIRECTION('center_axis',(1.,0.,0.));
#4794=DIRECTION('ref_axis',(0.,0.,-1.));
#4795=DIRECTION('center_axis',(1.,0.,0.));
#4796=DIRECTION('ref_axis',(0.,0.,-1.));
#4797=DIRECTION('center_axis',(1.,0.,0.));
#4798=DIRECTION('ref_axis',(0.,0.,-1.));
#4799=DIRECTION('',(1.,0.,0.));
#4800=DIRECTION('center_axis',(-1.,0.,0.));
#4801=DIRECTION('ref_axis',(0.,0.,1.));
#4802=DIRECTION('axis',(0.,0.,1.));
#4803=DIRECTION('refdir',(1.,0.,0.));
#4804=DIRECTION('center_axis',(1.,0.,0.));
#4805=DIRECTION('ref_axis',(0.,0.,-1.));
#4806=DIRECTION('center_axis',(-1.,0.,0.));
#4807=DIRECTION('ref_axis',(0.,1.22464679914735E-16,1.));
#4808=DIRECTION('center_axis',(0.,-1.,-1.22464679914735E-16));
#4809=DIRECTION('ref_axis',(0.,-1.22464679914735E-16,1.));
#4810=DIRECTION('center_axis',(1.,0.,0.));
#4811=DIRECTION('ref_axis',(0.,0.,1.));
#4812=DIRECTION('center_axis',(1.,0.,0.));
#4813=DIRECTION('ref_axis',(0.,0.,-1.));
#4814=DIRECTION('',(-0.999999956307574,3.62016965809512E-20,-0.000295609285927634));
#4815=DIRECTION('center_axis',(-1.,0.,0.));
#4816=DIRECTION('ref_axis',(0.,0.,1.));
#4817=DIRECTION('center_axis',(1.,0.,0.));
#4818=DIRECTION('ref_axis',(0.,0.,-1.));
#4819=DIRECTION('center_axis',(1.,0.,0.));
#4820=DIRECTION('ref_axis',(0.,0.,-1.));
#4821=DIRECTION('center_axis',(0.,-1.,-1.22464679914735E-16));
#4822=DIRECTION('ref_axis',(0.,-1.22464679914735E-16,1.));
#4823=DIRECTION('center_axis',(1.,0.,0.));
#4824=DIRECTION('ref_axis',(0.,1.22464679914735E-16,1.));
#4825=DIRECTION('center_axis',(-1.,0.,0.));
#4826=DIRECTION('ref_axis',(0.,0.,1.));
#4827=DIRECTION('axis',(0.,0.,1.));
#4828=DIRECTION('refdir',(1.,0.,0.));
#4829=DIRECTION('center_axis',(1.,0.,0.));
#4830=DIRECTION('ref_axis',(0.,0.,-1.));
#4831=DIRECTION('',(-1.,0.,0.));
#4832=DIRECTION('center_axis',(-1.,0.,0.));
#4833=DIRECTION('ref_axis',(0.,0.,-1.));
#4834=DIRECTION('',(-1.,0.,0.));
#4835=DIRECTION('center_axis',(-1.,0.,0.));
#4836=DIRECTION('ref_axis',(0.,0.,-1.));
#4837=DIRECTION('center_axis',(-1.,0.,0.));
#4838=DIRECTION('ref_axis',(0.,0.,-1.));
#4839=DIRECTION('center_axis',(1.,0.,0.));
#4840=DIRECTION('ref_axis',(0.,0.,-1.));
#4841=DIRECTION('',(-1.,0.,0.));
#4842=DIRECTION('center_axis',(1.,0.,0.));
#4843=DIRECTION('ref_axis',(0.,0.,-1.));
#4844=DIRECTION('',(-1.,0.,0.));
#4845=DIRECTION('center_axis',(1.,0.,0.));
#4846=DIRECTION('ref_axis',(0.,0.,-1.));
#4847=DIRECTION('',(-1.,0.,0.));
#4848=DIRECTION('center_axis',(1.,0.,0.));
#4849=DIRECTION('ref_axis',(0.,0.,-1.));
#4850=DIRECTION('',(-1.,0.,0.));
#4851=DIRECTION('center_axis',(1.,0.,0.));
#4852=DIRECTION('ref_axis',(0.,0.,-1.));
#4853=DIRECTION('',(-1.,0.,0.));
#4854=DIRECTION('center_axis',(1.,0.,0.));
#4855=DIRECTION('ref_axis',(0.,0.,-1.));
#4856=DIRECTION('',(-1.,0.,0.));
#4857=DIRECTION('center_axis',(1.,0.,0.));
#4858=DIRECTION('ref_axis',(0.,0.,-1.));
#4859=DIRECTION('',(-1.,0.,0.));
#4860=DIRECTION('center_axis',(1.,0.,0.));
#4861=DIRECTION('ref_axis',(0.,0.,-1.));
#4862=DIRECTION('',(-1.,0.,0.));
#4863=DIRECTION('center_axis',(1.,0.,0.));
#4864=DIRECTION('ref_axis',(0.,0.,-1.));
#4865=DIRECTION('',(-1.,0.,0.));
#4866=DIRECTION('center_axis',(1.,0.,0.));
#4867=DIRECTION('ref_axis',(0.,0.,-1.));
#4868=DIRECTION('',(-1.,0.,0.));
#4869=DIRECTION('center_axis',(1.,0.,0.));
#4870=DIRECTION('ref_axis',(0.,0.,-1.));
#4871=DIRECTION('',(-1.,0.,0.));
#4872=DIRECTION('center_axis',(1.,0.,0.));
#4873=DIRECTION('ref_axis',(0.,0.,-1.));
#4874=DIRECTION('',(-1.,0.,0.));
#4875=DIRECTION('center_axis',(1.,0.,0.));
#4876=DIRECTION('ref_axis',(0.,-0.999641738703431,0.0267655420640338));
#4877=DIRECTION('',(-1.,0.,0.));
#4878=DIRECTION('center_axis',(-1.,0.,0.));
#4879=DIRECTION('ref_axis',(0.,9.28774802075533E-14,-1.));
#4880=DIRECTION('center_axis',(1.,0.,0.));
#4881=DIRECTION('ref_axis',(0.,-0.999641738703431,0.0267655420640338));
#4882=DIRECTION('',(-1.,0.,0.));
#4883=DIRECTION('center_axis',(1.,0.,0.));
#4884=DIRECTION('ref_axis',(0.,-0.999641738703431,0.0267655420640338));
#4885=DIRECTION('',(-1.,0.,0.));
#4886=DIRECTION('center_axis',(1.,0.,0.));
#4887=DIRECTION('ref_axis',(0.,-0.999641738703431,0.0267655420640338));
#4888=DIRECTION('',(-1.,0.,0.));
#4889=DIRECTION('center_axis',(1.,0.,0.));
#4890=DIRECTION('ref_axis',(0.,-0.999641738703431,0.0267655420640338));
#4891=DIRECTION('',(-1.,0.,0.));
#4892=DIRECTION('center_axis',(1.,0.,0.));
#4893=DIRECTION('ref_axis',(0.,-0.999641738703431,0.0267655420640338));
#4894=DIRECTION('',(-1.,0.,0.));
#4895=DIRECTION('center_axis',(1.,0.,0.));
#4896=DIRECTION('ref_axis',(0.,-0.999641738703431,0.0267655420640338));
#4897=DIRECTION('',(-1.,0.,0.));
#4898=DIRECTION('center_axis',(1.,0.,0.));
#4899=DIRECTION('ref_axis',(0.,-0.999641738703431,0.0267655420640338));
#4900=DIRECTION('',(-1.,0.,0.));
#4901=DIRECTION('center_axis',(1.,0.,0.));
#4902=DIRECTION('ref_axis',(0.,-0.999641738703431,0.0267655420640338));
#4903=DIRECTION('',(-1.,0.,0.));
#4904=DIRECTION('center_axis',(1.,0.,0.));
#4905=DIRECTION('ref_axis',(0.,-0.999641738703431,0.0267655420640338));
#4906=DIRECTION('',(-1.,0.,0.));
#4907=DIRECTION('center_axis',(1.,0.,0.));
#4908=DIRECTION('ref_axis',(0.,-0.999641738703431,0.0267655420640338));
#4909=DIRECTION('',(-1.,0.,0.));
#4910=DIRECTION('center_axis',(1.,0.,0.));
#4911=DIRECTION('ref_axis',(0.,-0.999641738703431,0.0267655420640338));
#4912=DIRECTION('',(-1.,0.,0.));
#4913=DIRECTION('center_axis',(1.,0.,0.));
#4914=DIRECTION('ref_axis',(0.,-0.999641738703431,0.0267655420640338));
#4915=DIRECTION('',(-1.,0.,0.));
#4916=DIRECTION('center_axis',(1.,0.,0.));
#4917=DIRECTION('ref_axis',(0.,-0.999641738703431,0.0267655420640338));
#4918=DIRECTION('center_axis',(1.,0.,0.));
#4919=DIRECTION('ref_axis',(0.,9.28774802075533E-14,-1.));
#4920=DIRECTION('center_axis',(0.,1.,0.));
#4921=DIRECTION('ref_axis',(1.,0.,0.));
#4922=DIRECTION('center_axis',(0.,1.,0.));
#4923=DIRECTION('ref_axis',(1.,0.,0.));
#4924=DIRECTION('',(0.,1.,0.));
#4925=DIRECTION('center_axis',(0.,1.,0.));
#4926=DIRECTION('ref_axis',(1.,0.,0.));
#4927=DIRECTION('center_axis',(1.,0.,0.));
#4928=DIRECTION('ref_axis',(0.,0.,-1.));
#4929=DIRECTION('center_axis',(-1.,0.,0.));
#4930=DIRECTION('ref_axis',(0.,0.,-1.));
#4931=DIRECTION('center_axis',(-1.,0.,0.));
#4932=DIRECTION('ref_axis',(0.,0.,1.));
#4933=DIRECTION('center_axis',(1.,0.,0.));
#4934=DIRECTION('ref_axis',(0.,1.22464679914735E-16,1.));
#4935=DIRECTION('center_axis',(-1.,0.,0.));
#4936=DIRECTION('ref_axis',(0.,1.22464679914735E-16,1.));
#4937=DIRECTION('center_axis',(1.,0.,0.));
#4938=DIRECTION('ref_axis',(0.,0.,-1.));
#4939=DIRECTION('center_axis',(-1.,0.,0.));
#4940=DIRECTION('ref_axis',(0.,0.,-1.));
#4941=DIRECTION('center_axis',(0.,-1.,-1.22464679914735E-16));
#4942=DIRECTION('ref_axis',(0.,-1.22464679914735E-16,1.));
#4943=DIRECTION('center_axis',(1.,0.,0.));
#4944=DIRECTION('ref_axis',(0.,0.,1.));
#4945=DIRECTION('center_axis',(1.,0.,0.));
#4946=DIRECTION('ref_axis',(0.,0.,-1.));
#4947=DIRECTION('',(-0.999999956307574,3.62016965809699E-20,-0.000295609285927787));
#4948=DIRECTION('center_axis',(-1.,0.,0.));
#4949=DIRECTION('ref_axis',(0.,0.,1.));
#4950=DIRECTION('center_axis',(1.,0.,0.));
#4951=DIRECTION('ref_axis',(0.,0.,-1.));
#4952=DIRECTION('center_axis',(0.,-1.,-1.22464679914735E-16));
#4953=DIRECTION('ref_axis',(0.,-1.22464679914735E-16,1.));
#4954=DIRECTION('center_axis',(-1.,0.,0.));
#4955=DIRECTION('ref_axis',(0.,0.,1.));
#4956=DIRECTION('center_axis',(1.,0.,0.));
#4957=DIRECTION('ref_axis',(0.,1.22464679914735E-16,1.));
#4958=DIRECTION('center_axis',(1.,0.,0.));
#4959=DIRECTION('ref_axis',(0.,0.,-1.));
#4960=DIRECTION('center_axis',(1.,0.,0.));
#4961=DIRECTION('ref_axis',(0.,0.,-1.));
#4962=DIRECTION('center_axis',(1.,0.,0.));
#4963=DIRECTION('ref_axis',(0.,0.,-1.));
#4964=DIRECTION('center_axis',(-1.,0.,0.));
#4965=DIRECTION('ref_axis',(0.,1.22464679914735E-16,1.));
#4966=DIRECTION('center_axis',(0.,-1.,-1.22464679914735E-16));
#4967=DIRECTION('ref_axis',(0.,-1.22464679914735E-16,1.));
#4968=DIRECTION('center_axis',(1.,0.,0.));
#4969=DIRECTION('ref_axis',(0.,1.22464679914735E-16,1.));
#4970=DIRECTION('center_axis',(1.,0.,0.));
#4971=DIRECTION('ref_axis',(0.,0.,-1.));
#4972=DIRECTION('',(-1.,0.,0.));
#4973=DIRECTION('center_axis',(1.,0.,0.));
#4974=DIRECTION('ref_axis',(0.,0.,-1.));
#4975=DIRECTION('center_axis',(1.,0.,0.));
#4976=DIRECTION('ref_axis',(0.,0.,-1.));
#4977=DIRECTION('center_axis',(1.,0.,0.));
#4978=DIRECTION('ref_axis',(0.,0.,-1.));
#4979=DIRECTION('center_axis',(-1.,0.,0.));
#4980=DIRECTION('ref_axis',(0.,1.22464679914735E-16,1.));
#4981=DIRECTION('center_axis',(0.,-1.,-1.22464679914735E-16));
#4982=DIRECTION('ref_axis',(0.,-1.22464679914735E-16,1.));
#4983=DIRECTION('center_axis',(1.,0.,0.));
#4984=DIRECTION('ref_axis',(0.,0.,1.));
#4985=DIRECTION('center_axis',(1.,0.,0.));
#4986=DIRECTION('ref_axis',(0.,0.,-1.));
#4987=DIRECTION('',(-0.999999956307574,3.62016965808668E-20,-0.000295609285926945));
#4988=DIRECTION('center_axis',(-1.,0.,0.));
#4989=DIRECTION('ref_axis',(0.,0.,1.));
#4990=DIRECTION('center_axis',(1.,0.,0.));
#4991=DIRECTION('ref_axis',(0.,0.,-1.));
#4992=DIRECTION('center_axis',(1.,0.,0.));
#4993=DIRECTION('ref_axis',(0.,0.,-1.));
#4994=DIRECTION('center_axis',(0.,-1.,-1.22464679914735E-16));
#4995=DIRECTION('ref_axis',(0.,-1.22464679914735E-16,1.));
#4996=DIRECTION('center_axis',(1.,0.,0.));
#4997=DIRECTION('ref_axis',(0.,1.22464679914735E-16,1.));
#4998=DIRECTION('center_axis',(-1.,0.,0.));
#4999=DIRECTION('ref_axis',(0.,0.,1.));
#5000=DIRECTION('center_axis',(1.,0.,0.));
#5001=DIRECTION('ref_axis',(0.,0.,-1.));
#5002=DIRECTION('center_axis',(1.,0.,0.));
#5003=DIRECTION('ref_axis',(0.,0.,-1.));
#5004=DIRECTION('center_axis',(-1.,0.,0.));
#5005=DIRECTION('ref_axis',(0.,1.22464679914735E-16,1.));
#5006=DIRECTION('center_axis',(0.,-1.,-1.22464679914735E-16));
#5007=DIRECTION('ref_axis',(0.,-1.22464679914735E-16,1.));
#5008=DIRECTION('center_axis',(1.,0.,0.));
#5009=DIRECTION('ref_axis',(0.,0.,1.));
#5010=DIRECTION('center_axis',(1.,0.,0.));
#5011=DIRECTION('ref_axis',(0.,0.,-1.));
#5012=DIRECTION('',(-0.999999956307574,3.62016965808707E-20,-0.000295609285926977));
#5013=DIRECTION('center_axis',(-1.,0.,0.));
#5014=DIRECTION('ref_axis',(0.,0.,1.));
#5015=DIRECTION('center_axis',(1.,0.,0.));
#5016=DIRECTION('ref_axis',(0.,0.,-1.));
#5017=DIRECTION('center_axis',(1.,0.,0.));
#5018=DIRECTION('ref_axis',(0.,0.,-1.));
#5019=DIRECTION('center_axis',(1.,0.,0.));
#5020=DIRECTION('ref_axis',(0.,0.,-1.));
#5021=DIRECTION('center_axis',(0.,-1.,-1.22464679914735E-16));
#5022=DIRECTION('ref_axis',(0.,-1.22464679914735E-16,1.));
#5023=DIRECTION('center_axis',(1.,0.,0.));
#5024=DIRECTION('ref_axis',(0.,0.,-1.));
#5025=DIRECTION('center_axis',(0.,-1.,-1.22464679914735E-16));
#5026=DIRECTION('ref_axis',(0.,-1.22464679914735E-16,1.));
#5027=DIRECTION('center_axis',(1.,0.,0.));
#5028=DIRECTION('ref_axis',(0.,0.,1.));
#5029=DIRECTION('center_axis',(1.,0.,0.));
#5030=DIRECTION('ref_axis',(0.,0.,-1.));
#5031=DIRECTION('',(-0.999999956307574,3.62016965808673E-20,-0.000295609285926949));
#5032=DIRECTION('center_axis',(-1.,0.,0.));
#5033=DIRECTION('ref_axis',(0.,0.,1.));
#5034=DIRECTION('center_axis',(1.,0.,0.));
#5035=DIRECTION('ref_axis',(0.,0.,-1.));
#5036=DIRECTION('center_axis',(0.,-1.,-1.22464679914735E-16));
#5037=DIRECTION('ref_axis',(0.,-1.22464679914735E-16,1.));
#5038=DIRECTION('center_axis',(1.,0.,0.));
#5039=DIRECTION('ref_axis',(0.,1.22464679914735E-16,1.));
#5040=DIRECTION('center_axis',(-1.,0.,0.));
#5041=DIRECTION('ref_axis',(0.,0.,1.));
#5042=DIRECTION('center_axis',(1.,0.,0.));
#5043=DIRECTION('ref_axis',(0.,0.,-1.));
#5044=DIRECTION('center_axis',(1.,0.,0.));
#5045=DIRECTION('ref_axis',(0.,0.,-1.));
#5046=DIRECTION('center_axis',(-1.,0.,0.));
#5047=DIRECTION('ref_axis',(0.,1.22464679914735E-16,1.));
#5048=DIRECTION('center_axis',(0.,-1.,-1.22464679914735E-16));
#5049=DIRECTION('ref_axis',(0.,-1.22464679914735E-16,1.));
#5050=DIRECTION('center_axis',(1.,0.,0.));
#5051=DIRECTION('ref_axis',(0.,0.,1.));
#5052=DIRECTION('center_axis',(1.,0.,0.));
#5053=DIRECTION('ref_axis',(0.,0.,-1.));
#5054=DIRECTION('',(-0.999999956307574,3.62016965810123E-20,-0.000295609285928133));
#5055=DIRECTION('center_axis',(-1.,0.,0.));
#5056=DIRECTION('ref_axis',(0.,0.,1.));
#5057=DIRECTION('center_axis',(1.,0.,0.));
#5058=DIRECTION('ref_axis',(0.,0.,-1.));
#5059=DIRECTION('center_axis',(1.,0.,0.));
#5060=DIRECTION('ref_axis',(0.,0.,-1.));
#5061=DIRECTION('center_axis',(1.,0.,0.));
#5062=DIRECTION('ref_axis',(0.,0.,-1.));
#5063=DIRECTION('center_axis',(0.,-1.,-1.22464679914735E-16));
#5064=DIRECTION('ref_axis',(0.,-1.22464679914735E-16,1.));
#5065=DIRECTION('center_axis',(1.,0.,0.));
#5066=DIRECTION('ref_axis',(0.,1.22464679914735E-16,1.));
#5067=DIRECTION('center_axis',(-1.,0.,0.));
#5068=DIRECTION('ref_axis',(0.,0.,1.));
#5069=DIRECTION('center_axis',(1.,0.,0.));
#5070=DIRECTION('ref_axis',(0.,0.,-1.));
#5071=DIRECTION('center_axis',(1.,0.,0.));
#5072=DIRECTION('ref_axis',(0.,0.,-1.));
#5073=DIRECTION('center_axis',(-1.,0.,0.));
#5074=DIRECTION('ref_axis',(0.,1.22464679914735E-16,1.));
#5075=DIRECTION('center_axis',(0.,-1.,-1.22464679914735E-16));
#5076=DIRECTION('ref_axis',(0.,-1.22464679914735E-16,1.));
#5077=DIRECTION('center_axis',(1.,0.,0.));
#5078=DIRECTION('ref_axis',(0.,1.22464679914735E-16,1.));
#5079=DIRECTION('center_axis',(-1.,0.,0.));
#5080=DIRECTION('ref_axis',(0.,0.,1.));
#5081=DIRECTION('center_axis',(1.,0.,0.));
#5082=DIRECTION('ref_axis',(0.,0.,-1.));
#5083=DIRECTION('',(-1.,0.,0.));
#5084=DIRECTION('center_axis',(1.,0.,0.));
#5085=DIRECTION('ref_axis',(0.,0.,-1.));
#5086=DIRECTION('',(-1.,0.,0.));
#5087=DIRECTION('center_axis',(1.,0.,0.));
#5088=DIRECTION('ref_axis',(0.,0.,-1.));
#5089=DIRECTION('',(-1.,0.,0.));
#5090=DIRECTION('axis',(0.,0.,1.));
#5091=DIRECTION('refdir',(1.,0.,0.));
#5092=DIRECTION('center_axis',(1.,0.,0.));
#5093=DIRECTION('ref_axis',(0.,1.,0.));
#5094=DIRECTION('center_axis',(1.,0.,0.));
#5095=DIRECTION('ref_axis',(0.,0.,-1.));
#5096=DIRECTION('',(-1.,0.,0.));
#5097=DIRECTION('center_axis',(1.,0.,0.));
#5098=DIRECTION('ref_axis',(0.,0.,-1.));
#5099=DIRECTION('center_axis',(1.,0.,0.));
#5100=DIRECTION('ref_axis',(0.,0.,-1.));
#5101=DIRECTION('center_axis',(1.,0.,0.));
#5102=DIRECTION('ref_axis',(0.,0.,-1.));
#5103=DIRECTION('center_axis',(1.,0.,0.));
#5104=DIRECTION('ref_axis',(0.,1.,0.));
#5105=DIRECTION('center_axis',(1.,0.,0.));
#5106=DIRECTION('ref_axis',(0.,0.,-1.));
#5107=DIRECTION('',(1.,0.,0.));
#5108=DIRECTION('center_axis',(-1.,0.,0.));
#5109=DIRECTION('ref_axis',(0.,0.,1.));
#5110=DIRECTION('',(0.,0.,1.));
#5111=DIRECTION('',(1.,0.,0.));
#5112=DIRECTION('',(0.,0.,1.));
#5113=DIRECTION('',(1.,0.,0.));
#5114=DIRECTION('',(0.,0.,1.));
#5115=DIRECTION('',(1.,0.,0.));
#5116=DIRECTION('',(0.,0.,1.));
#5117=DIRECTION('',(1.,0.,0.));
#5118=DIRECTION('',(0.,0.,1.));
#5119=DIRECTION('',(1.,0.,0.));
#5120=DIRECTION('',(0.,0.,1.));
#5121=DIRECTION('',(1.,0.,0.));
#5122=DIRECTION('',(0.,0.,1.));
#5123=DIRECTION('',(1.,0.,0.));
#5124=DIRECTION('',(0.,0.,1.));
#5125=DIRECTION('',(1.,0.,0.));
#5126=DIRECTION('',(0.,0.,1.));
#5127=DIRECTION('',(1.,0.,0.));
#5128=DIRECTION('',(0.,0.,1.));
#5129=DIRECTION('',(1.,0.,0.));
#5130=CARTESIAN_POINT('',(0.,0.,0.));
#5131=CARTESIAN_POINT('',(0.,0.,0.));
#5132=CARTESIAN_POINT('Ctrl Pts',(82.4430005297901,1.97158113240038,3.97043534620108));
#5133=CARTESIAN_POINT('Ctrl Pts',(88.2030005297901,1.97158113240038,3.97043534620108));
#5134=CARTESIAN_POINT('Ctrl Pts',(82.4430005297901,2.29671111436096,3.77621792657108));
#5135=CARTESIAN_POINT('Ctrl Pts',(88.2030005297901,2.29671111436096,3.77621792657108));
#5136=CARTESIAN_POINT('Ctrl Pts',(82.4430005297901,2.59552275281558,3.54102114079632));
#5137=CARTESIAN_POINT('Ctrl Pts',(88.2030005297901,2.59552275281558,3.54102114079632));
#5138=CARTESIAN_POINT('Ctrl Pts',(82.4430005297901,3.11908576775695,3.00435277140383));
#5139=CARTESIAN_POINT('Ctrl Pts',(88.2030005297901,3.11908576775695,3.00435277140383));
#5140=CARTESIAN_POINT('Ctrl Pts',(82.4430005297901,3.34301024132503,2.70651491388494));
#5141=CARTESIAN_POINT('Ctrl Pts',(88.2030005297901,3.34301024132503,2.70651491388494));
#5142=CARTESIAN_POINT('Ctrl Pts',(82.4430005297901,3.79251211736076,1.90981794028965));
#5143=CARTESIAN_POINT('Ctrl Pts',(88.2030005297901,3.79251211736076,1.90981794028965));
#5144=CARTESIAN_POINT('Ctrl Pts',(82.4430005297901,3.96610878107774,1.3893796287376));
#5145=CARTESIAN_POINT('Ctrl Pts',(88.2030005297901,3.96610878107774,1.3893796287376));
#5146=CARTESIAN_POINT('Ctrl Pts',(82.4430005297901,4.09877879619631,0.327978495265378));
#5147=CARTESIAN_POINT('Ctrl Pts',(88.2030005297901,4.09877879619631,0.327978495265378));
#5148=CARTESIAN_POINT('Ctrl Pts',(82.4430005297901,4.06307606785725,-0.201870082003989));
#5149=CARTESIAN_POINT('Ctrl Pts',(88.2030005297901,4.06307606785725,-0.201870082003989));
#5150=CARTESIAN_POINT('Ctrl Pts',(82.4430005297901,3.79206680758235,-1.20058842967181));
#5151=CARTESIAN_POINT('Ctrl Pts',(88.2030005297901,3.79206680758235,-1.20058842967181));
#5152=CARTESIAN_POINT('Ctrl Pts',(82.4430005297901,3.56572122172907,-1.66148594501202));
#5153=CARTESIAN_POINT('Ctrl Pts',(88.2030005297901,3.56572122172907,-1.66148594501202));
#5154=CARTESIAN_POINT('Ctrl Pts',(82.4430005297901,2.95711124459234,-2.45497912282895));
#5155=CARTESIAN_POINT('Ctrl Pts',(88.2030005297901,2.95711124459234,-2.45497912282895));
#5156=CARTESIAN_POINT('Ctrl Pts',(82.4430005297901,2.58595465431404,-2.78386901588456));
#5157=CARTESIAN_POINT('Ctrl Pts',(88.2030005297901,2.58595465431404,-2.78386901588456));
#5158=CARTESIAN_POINT('Ctrl Pts',(82.4430005297901,2.16151778945147,-3.03095833168073));
#5159=CARTESIAN_POINT('Ctrl Pts',(88.2030005297901,2.16151778945147,-3.03095833168073));
#5160=CARTESIAN_POINT('',(82.4430005297901,1.97158113240038,3.97043534620107));
#5161=CARTESIAN_POINT('',(82.4430005297901,2.16151778945147,-3.03095833168073));
#5162=CARTESIAN_POINT('Ctrl Pts',(82.4430005297901,1.97158113240038,3.97043534620108));
#5163=CARTESIAN_POINT('Ctrl Pts',(82.4430005297901,2.29671111436096,3.77621792657108));
#5164=CARTESIAN_POINT('Ctrl Pts',(82.4430005297901,2.59552275281558,3.54102114079632));
#5165=CARTESIAN_POINT('Ctrl Pts',(82.4430005297901,3.11908576775695,3.00435277140383));
#5166=CARTESIAN_POINT('Ctrl Pts',(82.4430005297901,3.34301024132503,2.70651491388494));
#5167=CARTESIAN_POINT('Ctrl Pts',(82.4430005297901,3.79251211736076,1.90981794028965));
#5168=CARTESIAN_POINT('Ctrl Pts',(82.4430005297901,3.96610878107774,1.3893796287376));
#5169=CARTESIAN_POINT('Ctrl Pts',(82.4430005297901,4.09877879619631,0.327978495265378));
#5170=CARTESIAN_POINT('Ctrl Pts',(82.4430005297901,4.06307606785725,-0.201870082003989));
#5171=CARTESIAN_POINT('Ctrl Pts',(82.4430005297901,3.79206680758235,-1.20058842967181));
#5172=CARTESIAN_POINT('Ctrl Pts',(82.4430005297901,3.56572122172907,-1.66148594501202));
#5173=CARTESIAN_POINT('Ctrl Pts',(82.4430005297901,2.95711124459234,-2.45497912282895));
#5174=CARTESIAN_POINT('Ctrl Pts',(82.4430005297901,2.58595465431404,-2.78386901588456));
#5175=CARTESIAN_POINT('Ctrl Pts',(82.4430005297901,2.16151778945147,-3.03095833168073));
#5176=CARTESIAN_POINT('',(86.4430005297901,2.16151778945147,-3.03095833168073));
#5177=CARTESIAN_POINT('',(82.4430005297901,2.16151778945147,-3.03095833168073));
#5178=CARTESIAN_POINT('',(86.4430005297901,1.97158113240038,3.97043534620107));
#5179=CARTESIAN_POINT('Ctrl Pts',(86.4430005297901,1.97158113240038,3.97043534620108));
#5180=CARTESIAN_POINT('Ctrl Pts',(86.4430005297901,2.29671111436096,3.77621792657108));
#5181=CARTESIAN_POINT('Ctrl Pts',(86.4430005297901,2.59552275281558,3.54102114079632));
#5182=CARTESIAN_POINT('Ctrl Pts',(86.4430005297901,3.11908576775695,3.00435277140383));
#5183=CARTESIAN_POINT('Ctrl Pts',(86.4430005297901,3.34301024132503,2.70651491388494));
#5184=CARTESIAN_POINT('Ctrl Pts',(86.4430005297901,3.79251211736076,1.90981794028965));
#5185=CARTESIAN_POINT('Ctrl Pts',(86.4430005297901,3.96610878107774,1.3893796287376));
#5186=CARTESIAN_POINT('Ctrl Pts',(86.4430005297901,4.09877879619631,0.327978495265378));
#5187=CARTESIAN_POINT('Ctrl Pts',(86.4430005297901,4.06307606785725,-0.201870082003989));
#5188=CARTESIAN_POINT('Ctrl Pts',(86.4430005297901,3.79206680758235,-1.20058842967181));
#5189=CARTESIAN_POINT('Ctrl Pts',(86.4430005297901,3.56572122172907,-1.66148594501202));
#5190=CARTESIAN_POINT('Ctrl Pts',(86.4430005297901,2.95711124459234,-2.45497912282895));
#5191=CARTESIAN_POINT('Ctrl Pts',(86.4430005297901,2.58595465431404,-2.78386901588456));
#5192=CARTESIAN_POINT('Ctrl Pts',(86.4430005297901,2.16151778945147,-3.03095833168073));
#5193=CARTESIAN_POINT('',(82.4430005297901,1.97158113240038,3.97043534620107));
#5194=CARTESIAN_POINT('Origin',(82.4430005297901,-2.77555756156289E-16,
5.55111512312578E-16));
#5195=CARTESIAN_POINT('',(82.4430005297901,-1.97158113240039,3.97043534620107));
#5196=CARTESIAN_POINT('Origin',(82.4430005297901,-2.77555756156289E-16,
5.55111512312578E-16));
#5197=CARTESIAN_POINT('',(86.4430005297901,-1.97158113240039,3.97043534620107));
#5198=CARTESIAN_POINT('Origin',(86.4430005297901,-2.77555756156289E-16,
5.55111512312578E-16));
#5199=CARTESIAN_POINT('',(82.4430005297901,-1.97158113240039,3.97043534620107));
#5200=CARTESIAN_POINT('Ctrl Pts',(82.4430005297901,-2.16151778945139,-3.03095833168078));
#5201=CARTESIAN_POINT('Ctrl Pts',(88.2030005297901,-2.16151778945139,-3.03095833168078));
#5202=CARTESIAN_POINT('Ctrl Pts',(82.4430005297901,-2.4417969811413,-2.86779155838698));
#5203=CARTESIAN_POINT('Ctrl Pts',(88.2030005297901,-2.4417969811413,-2.86779155838698));
#5204=CARTESIAN_POINT('Ctrl Pts',(82.4430005297901,-2.69946597133354,-2.66855779259647));
#5205=CARTESIAN_POINT('Ctrl Pts',(88.2030005297901,-2.69946597133354,-2.66855779259647));
#5206=CARTESIAN_POINT('Ctrl Pts',(82.4430005297901,-3.16313807023027,-2.20413689736136));
#5207=CARTESIAN_POINT('Ctrl Pts',(88.2030005297901,-3.16313807023027,-2.20413689736136));
#5208=CARTESIAN_POINT('Ctrl Pts',(82.4430005297901,-3.36582061002206,-1.93954623621156));
#5209=CARTESIAN_POINT('Ctrl Pts',(88.2030005297901,-3.36582061002206,-1.93954623621156));
#5210=CARTESIAN_POINT('Ctrl Pts',(82.4430005297901,-3.7905877946382,-1.20735040930033));
#5211=CARTESIAN_POINT('Ctrl Pts',(88.2030005297901,-3.7905877946382,-1.20735040930033));
#5212=CARTESIAN_POINT('Ctrl Pts',(82.4430005297901,-3.95787261855977,-0.715467908482556));
#5213=CARTESIAN_POINT('Ctrl Pts',(88.2030005297901,-3.95787261855977,-0.715467908482556));
#5214=CARTESIAN_POINT('Ctrl Pts',(82.4430005297901,-4.0999785741866,0.321696095215354));
#5215=CARTESIAN_POINT('Ctrl Pts',(88.2030005297901,-4.0999785741866,0.321696095215354));
#5216=CARTESIAN_POINT('Ctrl Pts',(82.4430005297901,-4.06691955087291,0.857794436836504));
#5217=CARTESIAN_POINT('Ctrl Pts',(88.2030005297901,-4.06691955087291,0.857794436836504));
#5218=CARTESIAN_POINT('Ctrl Pts',(82.4430005297901,-3.79581350913489,1.90493582172488));
#5219=CARTESIAN_POINT('Ctrl Pts',(88.2030005297901,-3.79581350913489,1.90493582172488));
#5220=CARTESIAN_POINT('Ctrl Pts',(82.4430005297901,-3.55404702294629,2.40416273654669));
#5221=CARTESIAN_POINT('Ctrl Pts',(88.2030005297901,-3.55404702294629,2.40416273654669));
#5222=CARTESIAN_POINT('Ctrl Pts',(82.4430005297901,-2.88474862400959,3.29779955123577));
#5223=CARTESIAN_POINT('Ctrl Pts',(88.2030005297901,-2.88474862400959,3.29779955123577));
#5224=CARTESIAN_POINT('Ctrl Pts',(82.4430005297901,-2.45846445810197,3.67959405679301));
#5225=CARTESIAN_POINT('Ctrl Pts',(88.2030005297901,-2.45846445810197,3.67959405679301));
#5226=CARTESIAN_POINT('Ctrl Pts',(82.4430005297901,-1.97158113240039,3.97043534620107));
#5227=CARTESIAN_POINT('Ctrl Pts',(88.2030005297901,-1.97158113240039,3.97043534620107));
#5228=CARTESIAN_POINT('',(82.4430005297901,-2.16151778945139,-3.03095833168078));
#5229=CARTESIAN_POINT('Ctrl Pts',(82.4430005297901,-2.16151778945139,-3.03095833168078));
#5230=CARTESIAN_POINT('Ctrl Pts',(82.4430005297901,-2.4417969811413,-2.86779155838698));
#5231=CARTESIAN_POINT('Ctrl Pts',(82.4430005297901,-2.69946597133354,-2.66855779259647));
#5232=CARTESIAN_POINT('Ctrl Pts',(82.4430005297901,-3.16313807023027,-2.20413689736136));
#5233=CARTESIAN_POINT('Ctrl Pts',(82.4430005297901,-3.36582061002206,-1.93954623621156));
#5234=CARTESIAN_POINT('Ctrl Pts',(82.4430005297901,-3.7905877946382,-1.20735040930033));
#5235=CARTESIAN_POINT('Ctrl Pts',(82.4430005297901,-3.95787261855977,-0.715467908482556));
#5236=CARTESIAN_POINT('Ctrl Pts',(82.4430005297901,-4.0999785741866,0.321696095215354));
#5237=CARTESIAN_POINT('Ctrl Pts',(82.4430005297901,-4.06691955087291,0.857794436836504));
#5238=CARTESIAN_POINT('Ctrl Pts',(82.4430005297901,-3.79581350913489,1.90493582172488));
#5239=CARTESIAN_POINT('Ctrl Pts',(82.4430005297901,-3.55404702294629,2.40416273654669));
#5240=CARTESIAN_POINT('Ctrl Pts',(82.4430005297901,-2.88474862400959,3.29779955123577));
#5241=CARTESIAN_POINT('Ctrl Pts',(82.4430005297901,-2.45846445810197,3.67959405679301));
#5242=CARTESIAN_POINT('Ctrl Pts',(82.4430005297901,-1.97158113240039,3.97043534620107));
#5243=CARTESIAN_POINT('',(86.4430005297901,-2.16151778945139,-3.03095833168078));
#5244=CARTESIAN_POINT('Ctrl Pts',(86.4430005297901,-2.16151778945139,-3.03095833168078));
#5245=CARTESIAN_POINT('Ctrl Pts',(86.4430005297901,-2.4417969811413,-2.86779155838698));
#5246=CARTESIAN_POINT('Ctrl Pts',(86.4430005297901,-2.69946597133354,-2.66855779259647));
#5247=CARTESIAN_POINT('Ctrl Pts',(86.4430005297901,-3.16313807023027,-2.20413689736136));
#5248=CARTESIAN_POINT('Ctrl Pts',(86.4430005297901,-3.36582061002206,-1.93954623621156));
#5249=CARTESIAN_POINT('Ctrl Pts',(86.4430005297901,-3.7905877946382,-1.20735040930033));
#5250=CARTESIAN_POINT('Ctrl Pts',(86.4430005297901,-3.95787261855977,-0.715467908482556));
#5251=CARTESIAN_POINT('Ctrl Pts',(86.4430005297901,-4.0999785741866,0.321696095215354));
#5252=CARTESIAN_POINT('Ctrl Pts',(86.4430005297901,-4.06691955087291,0.857794436836504));
#5253=CARTESIAN_POINT('Ctrl Pts',(86.4430005297901,-3.79581350913489,1.90493582172488));
#5254=CARTESIAN_POINT('Ctrl Pts',(86.4430005297901,-3.55404702294629,2.40416273654669));
#5255=CARTESIAN_POINT('Ctrl Pts',(86.4430005297901,-2.88474862400959,3.29779955123577));
#5256=CARTESIAN_POINT('Ctrl Pts',(86.4430005297901,-2.45846445810197,3.67959405679301));
#5257=CARTESIAN_POINT('Ctrl Pts',(86.4430005297901,-1.97158113240039,3.97043534620107));
#5258=CARTESIAN_POINT('',(82.4430005297901,-2.16151778945139,-3.03095833168078));
#5259=CARTESIAN_POINT('Origin',(82.4430005297901,-2.77555756156289E-16,
5.55111512312578E-16));
#5260=CARTESIAN_POINT('Origin',(82.4430005297901,-2.77555756156289E-16,
5.55111512312578E-16));
#5261=CARTESIAN_POINT('Origin',(86.4430005297901,-2.77555756156289E-16,
5.55111512312578E-16));
#5262=CARTESIAN_POINT('Origin',(82.4430005297901,7.33246945257534,-3.33066907387547E-15));
#5263=CARTESIAN_POINT('',(82.4430005297901,7.33246945257534,-3.33066907387547E-15));
#5264=CARTESIAN_POINT('',(82.4430005297901,3.66623472628768,6.35010481840362));
#5265=CARTESIAN_POINT('',(82.4430005297901,7.33246945257534,-3.33066907387547E-15));
#5266=CARTESIAN_POINT('',(86.4430005297901,3.66623472628768,6.35010481840362));
#5267=CARTESIAN_POINT('',(82.4430005297901,3.66623472628768,6.35010481840362));
#5268=CARTESIAN_POINT('',(86.4430005297901,7.33246945257534,-3.33066907387547E-15));
#5269=CARTESIAN_POINT('',(86.4430005297901,7.33246945257534,-3.33066907387547E-15));
#5270=CARTESIAN_POINT('',(82.4430005297901,7.33246945257534,-3.33066907387547E-15));
#5271=CARTESIAN_POINT('Origin',(82.4430005297901,3.66623472628767,-6.35010481840363));
#5272=CARTESIAN_POINT('',(82.4430005297901,3.66623472628767,-6.35010481840363));
#5273=CARTESIAN_POINT('',(82.4430005297901,3.66623472628767,-6.35010481840363));
#5274=CARTESIAN_POINT('',(86.4430005297901,3.66623472628767,-6.35010481840363));
#5275=CARTESIAN_POINT('',(86.4430005297901,3.66623472628767,-6.35010481840363));
#5276=CARTESIAN_POINT('',(82.4430005297901,3.66623472628767,-6.35010481840363));
#5277=CARTESIAN_POINT('Origin',(82.4430005297901,-3.66623472628767,-6.35010481840362));
#5278=CARTESIAN_POINT('',(82.4430005297901,-3.66623472628767,-6.35010481840362));
#5279=CARTESIAN_POINT('',(82.4430005297901,-3.66623472628767,-6.35010481840362));
#5280=CARTESIAN_POINT('',(86.4430005297901,-3.66623472628767,-6.35010481840362));
#5281=CARTESIAN_POINT('',(86.4430005297901,-3.66623472628767,-6.35010481840362));
#5282=CARTESIAN_POINT('',(82.4430005297901,-3.66623472628767,-6.35010481840362));
#5283=CARTESIAN_POINT('Origin',(82.4430005297901,-7.33246945257535,2.77555756156289E-15));
#5284=CARTESIAN_POINT('',(82.4430005297901,-7.33246945257535,2.77555756156289E-15));
#5285=CARTESIAN_POINT('',(82.4430005297901,-7.33246945257535,2.77555756156289E-15));
#5286=CARTESIAN_POINT('',(86.4430005297901,-7.33246945257535,2.77555756156289E-15));
#5287=CARTESIAN_POINT('',(86.4430005297901,-7.33246945257535,2.77555756156289E-15));
#5288=CARTESIAN_POINT('',(82.4430005297901,-7.33246945257535,2.77555756156289E-15));
#5289=CARTESIAN_POINT('Origin',(82.4430005297901,-3.66623472628767,6.35010481840363));
#5290=CARTESIAN_POINT('',(82.4430005297901,-3.66623472628767,6.35010481840363));
#5291=CARTESIAN_POINT('',(82.4430005297901,-3.66623472628767,6.35010481840363));
#5292=CARTESIAN_POINT('',(86.4430005297901,-3.66623472628767,6.35010481840363));
#5293=CARTESIAN_POINT('',(86.4430005297901,-3.66623472628767,6.35010481840363));
#5294=CARTESIAN_POINT('',(82.4430005297901,-3.66623472628767,6.35010481840363));
#5295=CARTESIAN_POINT('Origin',(82.4430005297901,3.66623472628768,6.35010481840362));
#5296=CARTESIAN_POINT('',(82.4430005297901,3.66623472628768,6.35010481840362));
#5297=CARTESIAN_POINT('',(86.4430005297901,3.66623472628768,6.35010481840362));
#5298=CARTESIAN_POINT('Origin',(86.4430005297901,0.,0.));
#5299=CARTESIAN_POINT('Origin',(82.4430005297901,0.,0.));
#5300=CARTESIAN_POINT('',(0.,0.,0.));
#5301=CARTESIAN_POINT('Origin',(70.8,0.,0.));
#5302=CARTESIAN_POINT('',(70.8,4.64354390525168,0.999999999999997));
#5303=CARTESIAN_POINT('',(69.8,4.75,-1.64281711919618E-16));
#5304=CARTESIAN_POINT('Ctrl Pts',(70.8,4.64354390525168,0.999999999999997));
#5305=CARTESIAN_POINT('Ctrl Pts',(70.9259729879541,4.64354390525168,0.999999999999997));
#5306=CARTESIAN_POINT('Ctrl Pts',(71.0600756275793,4.64920215672275,0.974746883632144));
#5307=CARTESIAN_POINT('Ctrl Pts',(71.3063376808864,4.66945597411313,0.872578382964584));
#5308=CARTESIAN_POINT('Ctrl Pts',(71.4185308600728,4.68373916194669,0.79568270230026));
#5309=CARTESIAN_POINT('Ctrl Pts',(71.5956765832561,4.71040703090821,0.618536979117035));
#5310=CARTESIAN_POINT('Ctrl Pts',(71.672577053022,4.72455080089029,0.50634121101625));
#5311=CARTESIAN_POINT('Ctrl Pts',(71.774749031943,4.74448366225285,0.260070124891274));
#5312=CARTESIAN_POINT('Ctrl Pts',(71.8,4.75,0.125964285427863));
#5313=CARTESIAN_POINT('Ctrl Pts',(71.8,4.75,-0.125964285427863));
#5314=CARTESIAN_POINT('Ctrl Pts',(71.774749031943,4.74448366225285,-0.260070124891274));
#5315=CARTESIAN_POINT('Ctrl Pts',(71.672577053022,4.72455080089029,-0.50634121101625));
#5316=CARTESIAN_POINT('Ctrl Pts',(71.5956765832561,4.71040703090821,-0.618536979117036));
#5317=CARTESIAN_POINT('Ctrl Pts',(71.4185308600728,4.68373916194669,-0.79568270230026));
#5318=CARTESIAN_POINT('Ctrl Pts',(71.3063376808864,4.66945597411313,-0.872578382964578));
#5319=CARTESIAN_POINT('Ctrl Pts',(71.0600756275793,4.64920215672275,-0.97474688363214));
#5320=CARTESIAN_POINT('Ctrl Pts',(70.9259729879542,4.64354390525168,-0.999999999999996));
#5321=CARTESIAN_POINT('Ctrl Pts',(70.6740270120459,4.64354390525168,-0.999999999999996));
#5322=CARTESIAN_POINT('Ctrl Pts',(70.5399243724207,4.64920215672275,-0.974746883632144));
#5323=CARTESIAN_POINT('Ctrl Pts',(70.2936623191136,4.66945597411312,-0.872578382964589));
#5324=CARTESIAN_POINT('Ctrl Pts',(70.1814691399272,4.68373916194669,-0.79568270230026));
#5325=CARTESIAN_POINT('Ctrl Pts',(70.0043234167439,4.71040703090821,-0.618536979117036));
#5326=CARTESIAN_POINT('Ctrl Pts',(69.927422946978,4.72455080089029,-0.50634121101625));
#5327=CARTESIAN_POINT('Ctrl Pts',(69.825250968057,4.74448366225285,-0.260070124891274));
#5328=CARTESIAN_POINT('Ctrl Pts',(69.8,4.75,-0.125964285427863));
#5329=CARTESIAN_POINT('Ctrl Pts',(69.8,4.75,-4.5102810375397E-16));
#5330=CARTESIAN_POINT('Ctrl Pts',(69.8,4.75,-1.38777878078145E-16));
#5331=CARTESIAN_POINT('Ctrl Pts',(69.8,4.75,0.125964285427862));
#5332=CARTESIAN_POINT('Ctrl Pts',(69.825250968057,4.74448366225285,0.260070124891274));
#5333=CARTESIAN_POINT('Ctrl Pts',(69.927422946978,4.72455080089029,0.50634121101625));
#5334=CARTESIAN_POINT('Ctrl Pts',(70.0043234167439,4.71040703090821,0.618536979117035));
#5335=CARTESIAN_POINT('Ctrl Pts',(70.1814691399272,4.68373916194669,0.79568270230026));
#5336=CARTESIAN_POINT('Ctrl Pts',(70.2936623191136,4.66945597411313,0.872578382964584));
#5337=CARTESIAN_POINT('Ctrl Pts',(70.5399243724207,4.64920215672275,0.974746883632144));
#5338=CARTESIAN_POINT('Ctrl Pts',(70.6740270120459,4.64354390525168,0.999999999999997));
#5339=CARTESIAN_POINT('Ctrl Pts',(70.8,4.64354390525168,0.999999999999997));
#5340=CARTESIAN_POINT('',(69.8,7.528,1.22464679914735E-16));
#5341=CARTESIAN_POINT('',(69.8,0.,1.22464679914735E-16));
#5342=CARTESIAN_POINT('',(70.8,7.46128568009562,0.999999999999996));
#5343=CARTESIAN_POINT('Ctrl Pts',(70.8,7.46128568009562,0.999999999999996));
#5344=CARTESIAN_POINT('Ctrl Pts',(70.67427740833,7.46128568009562,0.999999999999996));
#5345=CARTESIAN_POINT('Ctrl Pts',(70.540277592139,7.46479131730875,0.974843846039383));
#5346=CARTESIAN_POINT('Ctrl Pts',(70.2939429842273,7.4774158197129,0.87274427752583));
#5347=CARTESIAN_POINT('Ctrl Pts',(70.1815953412657,7.48634826149692,0.795808903638806));
#5348=CARTESIAN_POINT('Ctrl Pts',(70.004192043259,7.50308579458968,0.618405605632101));
#5349=CARTESIAN_POINT('Ctrl Pts',(69.9272559270855,7.51198372319629,0.506057551996159));
#5350=CARTESIAN_POINT('Ctrl Pts',(69.8251558158403,7.5245291161451,0.259721549521743));
#5351=CARTESIAN_POINT('Ctrl Pts',(69.8,7.528,0.125721249577576));
#5352=CARTESIAN_POINT('Ctrl Pts',(69.8,7.528,-3.46944695195361E-16));
#5353=CARTESIAN_POINT('Ctrl Pts',(69.8,7.528,-6.93889390390723E-17));
#5354=CARTESIAN_POINT('Ctrl Pts',(69.8,7.528,-0.125721249577577));
#5355=CARTESIAN_POINT('Ctrl Pts',(69.8251558158403,7.5245291161451,-0.259721549521743));
#5356=CARTESIAN_POINT('Ctrl Pts',(69.9272559270855,7.51198372319629,-0.506057551996159));
#5357=CARTESIAN_POINT('Ctrl Pts',(70.004192043259,7.50308579458968,-0.618405605632101));
#5358=CARTESIAN_POINT('Ctrl Pts',(70.1815953412657,7.48634826149692,-0.795808903638806));
#5359=CARTESIAN_POINT('Ctrl Pts',(70.2939429842273,7.4774158197129,-0.87274427752583));
#5360=CARTESIAN_POINT('Ctrl Pts',(70.540277592139,7.46479131730875,-0.974843846039383));
#5361=CARTESIAN_POINT('Ctrl Pts',(70.67427740833,7.46128568009562,-0.999999999999996));
#5362=CARTESIAN_POINT('Ctrl Pts',(70.92572259167,7.46128568009562,-0.999999999999996));
#5363=CARTESIAN_POINT('Ctrl Pts',(71.059722407861,7.46479131730875,-0.974843846039383));
#5364=CARTESIAN_POINT('Ctrl Pts',(71.3060570157727,7.4774158197129,-0.87274427752583));
#5365=CARTESIAN_POINT('Ctrl Pts',(71.4184046587343,7.48634826149692,-0.795808903638806));
#5366=CARTESIAN_POINT('Ctrl Pts',(71.595807956741,7.50308579458968,-0.618405605632101));
#5367=CARTESIAN_POINT('Ctrl Pts',(71.6727440729145,7.51198372319629,-0.506057551996159));
#5368=CARTESIAN_POINT('Ctrl Pts',(71.7748441841597,7.5245291161451,-0.259721549521743));
#5369=CARTESIAN_POINT('Ctrl Pts',(71.8,7.528,-0.125721249577577));
#5370=CARTESIAN_POINT('Ctrl Pts',(71.8,7.528,0.125721249577577));
#5371=CARTESIAN_POINT('Ctrl Pts',(71.7748441841597,7.5245291161451,0.259721549521733));
#5372=CARTESIAN_POINT('Ctrl Pts',(71.6727440729145,7.51198372319629,0.50605755199615));
#5373=CARTESIAN_POINT('Ctrl Pts',(71.595807956741,7.50308579458968,0.618405605632101));
#5374=CARTESIAN_POINT('Ctrl Pts',(71.4184046587343,7.48634826149692,0.795808903638806));
#5375=CARTESIAN_POINT('Ctrl Pts',(71.3060570157727,7.4774158197129,0.87274427752583));
#5376=CARTESIAN_POINT('Ctrl Pts',(71.059722407861,7.46479131730875,0.974843846039383));
#5377=CARTESIAN_POINT('Ctrl Pts',(70.92572259167,7.46128568009562,0.999999999999996));
#5378=CARTESIAN_POINT('Ctrl Pts',(70.8,7.46128568009562,0.999999999999996));
#5379=CARTESIAN_POINT('Origin',(69.875,0.,0.));
#5380=CARTESIAN_POINT('',(67.25,-4.75,-5.81707229594993E-16));
#5381=CARTESIAN_POINT('Origin',(67.25,0.,0.));
#5382=CARTESIAN_POINT('',(72.5,-4.75,-5.81707229594993E-16));
#5383=CARTESIAN_POINT('',(69.875,-4.75,-5.81707229594993E-16));
#5384=CARTESIAN_POINT('Origin',(72.5,0.,0.));
#5385=CARTESIAN_POINT('Origin',(67.25,7.01,0.));
#5386=CARTESIAN_POINT('',(67.25,-7.01,-8.58477406202294E-16));
#5387=CARTESIAN_POINT('Origin',(67.25,0.,0.));
#5388=CARTESIAN_POINT('Origin',(67.57,0.,0.));
#5389=CARTESIAN_POINT('',(67.89,-7.528,-9.21914110398127E-16));
#5390=CARTESIAN_POINT('Origin',(67.89,0.,0.));
#5391=CARTESIAN_POINT('',(67.57,-7.269,-8.90195758300211E-16));
#5392=CARTESIAN_POINT('Origin',(74.14,0.,0.));
#5393=CARTESIAN_POINT('',(80.39,-7.528,-9.21914110398127E-16));
#5394=CARTESIAN_POINT('Origin',(80.39,0.,0.));
#5395=CARTESIAN_POINT('',(74.14,-7.528,-9.21914110398128E-16));
#5396=CARTESIAN_POINT('Origin',(80.915,0.,0.));
#5397=CARTESIAN_POINT('',(81.44,-6.42,-7.86223245052601E-16));
#5398=CARTESIAN_POINT('',(80.915,-6.974,8.54068677725364E-16));
#5399=CARTESIAN_POINT('Origin',(81.44,0.,0.));
#5400=CARTESIAN_POINT('Origin',(81.44,3.7,0.));
#5401=CARTESIAN_POINT('',(81.44,-3.7,-4.53119315684521E-16));
#5402=CARTESIAN_POINT('Origin',(81.44,0.,0.));
#5403=CARTESIAN_POINT('Origin',(80.44,0.,0.));
#5404=CARTESIAN_POINT('',(79.44,-3.7,-4.53119315684521E-16));
#5405=CARTESIAN_POINT('Origin',(79.44,0.,0.));
#5406=CARTESIAN_POINT('',(80.44,-3.7,-4.53119315684521E-16));
#5407=CARTESIAN_POINT('Origin',(79.44,2.204,0.));
#5408=CARTESIAN_POINT('',(79.44,-2.204,-2.69912154532077E-16));
#5409=CARTESIAN_POINT('Origin',(79.44,0.,0.));
#5410=CARTESIAN_POINT('Origin',(75.97,0.,0.));
#5411=CARTESIAN_POINT('',(72.5,-2.204,-2.69912154532077E-16));
#5412=CARTESIAN_POINT('Origin',(72.5,0.,0.));
#5413=CARTESIAN_POINT('',(75.97,-2.204,-2.69912154532077E-16));
#5414=CARTESIAN_POINT('Origin',(72.5,4.75,0.));
#5415=CARTESIAN_POINT('',(0.,0.,0.));
#5416=CARTESIAN_POINT('Ctrl Pts',(6.4430005297901,1.97158113240038,3.97043534620107));
#5417=CARTESIAN_POINT('Ctrl Pts',(12.2030005297901,1.97158113240038,3.97043534620107));
#5418=CARTESIAN_POINT('Ctrl Pts',(6.4430005297901,2.29671111436096,3.77621792657107));
#5419=CARTESIAN_POINT('Ctrl Pts',(12.2030005297901,2.29671111436096,3.77621792657107));
#5420=CARTESIAN_POINT('Ctrl Pts',(6.4430005297901,2.59552275281558,3.54102114079632));
#5421=CARTESIAN_POINT('Ctrl Pts',(12.2030005297901,2.59552275281558,3.54102114079632));
#5422=CARTESIAN_POINT('Ctrl Pts',(6.4430005297901,3.11908576775695,3.00435277140383));
#5423=CARTESIAN_POINT('Ctrl Pts',(12.2030005297901,3.11908576775695,3.00435277140383));
#5424=CARTESIAN_POINT('Ctrl Pts',(6.4430005297901,3.34301024132503,2.70651491388494));
#5425=CARTESIAN_POINT('Ctrl Pts',(12.2030005297901,3.34301024132503,2.70651491388494));
#5426=CARTESIAN_POINT('Ctrl Pts',(6.4430005297901,3.79251211736076,1.90981794028965));
#5427=CARTESIAN_POINT('Ctrl Pts',(12.2030005297901,3.79251211736076,1.90981794028965));
#5428=CARTESIAN_POINT('Ctrl Pts',(6.4430005297901,3.96610878107774,1.3893796287376));
#5429=CARTESIAN_POINT('Ctrl Pts',(12.2030005297901,3.96610878107774,1.3893796287376));
#5430=CARTESIAN_POINT('Ctrl Pts',(6.4430005297901,4.09877879619631,0.327978495265378));
#5431=CARTESIAN_POINT('Ctrl Pts',(12.2030005297901,4.09877879619631,0.327978495265378));
#5432=CARTESIAN_POINT('Ctrl Pts',(6.4430005297901,4.06307606785725,-0.201870082003989));
#5433=CARTESIAN_POINT('Ctrl Pts',(12.2030005297901,4.06307606785725,-0.201870082003989));
#5434=CARTESIAN_POINT('Ctrl Pts',(6.4430005297901,3.79206680758235,-1.20058842967181));
#5435=CARTESIAN_POINT('Ctrl Pts',(12.2030005297901,3.79206680758235,-1.20058842967181));
#5436=CARTESIAN_POINT('Ctrl Pts',(6.4430005297901,3.56572122172907,-1.66148594501202));
#5437=CARTESIAN_POINT('Ctrl Pts',(12.2030005297901,3.56572122172907,-1.66148594501202));
#5438=CARTESIAN_POINT('Ctrl Pts',(6.4430005297901,2.95711124459234,-2.45497912282895));
#5439=CARTESIAN_POINT('Ctrl Pts',(12.2030005297901,2.95711124459234,-2.45497912282895));
#5440=CARTESIAN_POINT('Ctrl Pts',(6.4430005297901,2.58595465431403,-2.78386901588454));
#5441=CARTESIAN_POINT('Ctrl Pts',(12.2030005297901,2.58595465431403,-2.78386901588454));
#5442=CARTESIAN_POINT('Ctrl Pts',(6.4430005297901,2.16151778945146,-3.03095833168072));
#5443=CARTESIAN_POINT('Ctrl Pts',(12.2030005297901,2.16151778945146,-3.03095833168072));
#5444=CARTESIAN_POINT('',(6.4430005297901,1.97158113240038,3.97043534620107));
#5445=CARTESIAN_POINT('',(6.4430005297901,2.16151778945147,-3.03095833168073));
#5446=CARTESIAN_POINT('Ctrl Pts',(6.4430005297901,1.97158113240038,3.97043534620107));
#5447=CARTESIAN_POINT('Ctrl Pts',(6.4430005297901,2.29671111436096,3.77621792657107));
#5448=CARTESIAN_POINT('Ctrl Pts',(6.4430005297901,2.59552275281558,3.54102114079632));
#5449=CARTESIAN_POINT('Ctrl Pts',(6.4430005297901,3.11908576775695,3.00435277140383));
#5450=CARTESIAN_POINT('Ctrl Pts',(6.4430005297901,3.34301024132503,2.70651491388494));
#5451=CARTESIAN_POINT('Ctrl Pts',(6.4430005297901,3.79251211736076,1.90981794028965));
#5452=CARTESIAN_POINT('Ctrl Pts',(6.4430005297901,3.96610878107774,1.3893796287376));
#5453=CARTESIAN_POINT('Ctrl Pts',(6.4430005297901,4.09877879619631,0.327978495265378));
#5454=CARTESIAN_POINT('Ctrl Pts',(6.4430005297901,4.06307606785725,-0.201870082003989));
#5455=CARTESIAN_POINT('Ctrl Pts',(6.4430005297901,3.79206680758235,-1.20058842967181));
#5456=CARTESIAN_POINT('Ctrl Pts',(6.4430005297901,3.56572122172907,-1.66148594501202));
#5457=CARTESIAN_POINT('Ctrl Pts',(6.4430005297901,2.95711124459234,-2.45497912282895));
#5458=CARTESIAN_POINT('Ctrl Pts',(6.4430005297901,2.58595465431403,-2.78386901588454));
#5459=CARTESIAN_POINT('Ctrl Pts',(6.4430005297901,2.16151778945146,-3.03095833168072));
#5460=CARTESIAN_POINT('',(10.4430005297901,2.16151778945147,-3.03095833168073));
#5461=CARTESIAN_POINT('',(6.4430005297901,2.16151778945147,-3.03095833168073));
#5462=CARTESIAN_POINT('',(10.4430005297901,1.97158113240038,3.97043534620107));
#5463=CARTESIAN_POINT('Ctrl Pts',(10.4430005297901,1.97158113240038,3.97043534620107));
#5464=CARTESIAN_POINT('Ctrl Pts',(10.4430005297901,2.29671111436096,3.77621792657107));
#5465=CARTESIAN_POINT('Ctrl Pts',(10.4430005297901,2.59552275281558,3.54102114079632));
#5466=CARTESIAN_POINT('Ctrl Pts',(10.4430005297901,3.11908576775695,3.00435277140383));
#5467=CARTESIAN_POINT('Ctrl Pts',(10.4430005297901,3.34301024132503,2.70651491388494));
#5468=CARTESIAN_POINT('Ctrl Pts',(10.4430005297901,3.79251211736076,1.90981794028965));
#5469=CARTESIAN_POINT('Ctrl Pts',(10.4430005297901,3.96610878107774,1.3893796287376));
#5470=CARTESIAN_POINT('Ctrl Pts',(10.4430005297901,4.09877879619631,0.327978495265378));
#5471=CARTESIAN_POINT('Ctrl Pts',(10.4430005297901,4.06307606785725,-0.201870082003989));
#5472=CARTESIAN_POINT('Ctrl Pts',(10.4430005297901,3.79206680758235,-1.20058842967181));
#5473=CARTESIAN_POINT('Ctrl Pts',(10.4430005297901,3.56572122172907,-1.66148594501202));
#5474=CARTESIAN_POINT('Ctrl Pts',(10.4430005297901,2.95711124459234,-2.45497912282895));
#5475=CARTESIAN_POINT('Ctrl Pts',(10.4430005297901,2.58595465431403,-2.78386901588454));
#5476=CARTESIAN_POINT('Ctrl Pts',(10.4430005297901,2.16151778945146,-3.03095833168072));
#5477=CARTESIAN_POINT('',(6.4430005297901,1.97158113240038,3.97043534620107));
#5478=CARTESIAN_POINT('Origin',(6.4430005297901,-2.77555756156289E-16,5.55111512312578E-16));
#5479=CARTESIAN_POINT('',(6.4430005297901,-1.97158113240039,3.97043534620107));
#5480=CARTESIAN_POINT('Origin',(6.4430005297901,-2.77555756156289E-16,5.55111512312578E-16));
#5481=CARTESIAN_POINT('',(10.4430005297901,-1.97158113240039,3.97043534620107));
#5482=CARTESIAN_POINT('Origin',(10.4430005297901,-2.77555756156289E-16,
5.55111512312578E-16));
#5483=CARTESIAN_POINT('',(6.4430005297901,-1.97158113240039,3.97043534620107));
#5484=CARTESIAN_POINT('Ctrl Pts',(6.4430005297901,-2.16151778945139,-3.03095833168078));
#5485=CARTESIAN_POINT('Ctrl Pts',(12.2030005297901,-2.16151778945139,-3.03095833168078));
#5486=CARTESIAN_POINT('Ctrl Pts',(6.4430005297901,-2.4417969811413,-2.86779155838698));
#5487=CARTESIAN_POINT('Ctrl Pts',(12.2030005297901,-2.4417969811413,-2.86779155838698));
#5488=CARTESIAN_POINT('Ctrl Pts',(6.4430005297901,-2.69946597133354,-2.66855779259647));
#5489=CARTESIAN_POINT('Ctrl Pts',(12.2030005297901,-2.69946597133354,-2.66855779259647));
#5490=CARTESIAN_POINT('Ctrl Pts',(6.4430005297901,-3.16313807023027,-2.20413689736136));
#5491=CARTESIAN_POINT('Ctrl Pts',(12.2030005297901,-3.16313807023027,-2.20413689736136));
#5492=CARTESIAN_POINT('Ctrl Pts',(6.4430005297901,-3.36582061002206,-1.93954623621156));
#5493=CARTESIAN_POINT('Ctrl Pts',(12.2030005297901,-3.36582061002206,-1.93954623621156));
#5494=CARTESIAN_POINT('Ctrl Pts',(6.4430005297901,-3.7905877946382,-1.20735040930033));
#5495=CARTESIAN_POINT('Ctrl Pts',(12.2030005297901,-3.7905877946382,-1.20735040930033));
#5496=CARTESIAN_POINT('Ctrl Pts',(6.4430005297901,-3.95787261855977,-0.715467908482556));
#5497=CARTESIAN_POINT('Ctrl Pts',(12.2030005297901,-3.95787261855977,-0.715467908482556));
#5498=CARTESIAN_POINT('Ctrl Pts',(6.4430005297901,-4.0999785741866,0.321696095215354));
#5499=CARTESIAN_POINT('Ctrl Pts',(12.2030005297901,-4.0999785741866,0.321696095215354));
#5500=CARTESIAN_POINT('Ctrl Pts',(6.4430005297901,-4.06691955087291,0.857794436836504));
#5501=CARTESIAN_POINT('Ctrl Pts',(12.2030005297901,-4.06691955087291,0.857794436836504));
#5502=CARTESIAN_POINT('Ctrl Pts',(6.4430005297901,-3.79581350913489,1.90493582172488));
#5503=CARTESIAN_POINT('Ctrl Pts',(12.2030005297901,-3.79581350913489,1.90493582172488));
#5504=CARTESIAN_POINT('Ctrl Pts',(6.4430005297901,-3.55404702294629,2.40416273654669));
#5505=CARTESIAN_POINT('Ctrl Pts',(12.2030005297901,-3.55404702294629,2.40416273654669));
#5506=CARTESIAN_POINT('Ctrl Pts',(6.4430005297901,-2.88474862400959,3.29779955123577));
#5507=CARTESIAN_POINT('Ctrl Pts',(12.2030005297901,-2.88474862400959,3.29779955123577));
#5508=CARTESIAN_POINT('Ctrl Pts',(6.4430005297901,-2.45846445810197,3.67959405679302));
#5509=CARTESIAN_POINT('Ctrl Pts',(12.2030005297901,-2.45846445810197,3.67959405679302));
#5510=CARTESIAN_POINT('Ctrl Pts',(6.4430005297901,-1.9715811324004,3.97043534620107));
#5511=CARTESIAN_POINT('Ctrl Pts',(12.2030005297901,-1.9715811324004,3.97043534620107));
#5512=CARTESIAN_POINT('',(6.4430005297901,-2.16151778945139,-3.03095833168078));
#5513=CARTESIAN_POINT('Ctrl Pts',(6.4430005297901,-2.16151778945139,-3.03095833168078));
#5514=CARTESIAN_POINT('Ctrl Pts',(6.4430005297901,-2.4417969811413,-2.86779155838698));
#5515=CARTESIAN_POINT('Ctrl Pts',(6.4430005297901,-2.69946597133354,-2.66855779259647));
#5516=CARTESIAN_POINT('Ctrl Pts',(6.4430005297901,-3.16313807023027,-2.20413689736136));
#5517=CARTESIAN_POINT('Ctrl Pts',(6.4430005297901,-3.36582061002206,-1.93954623621156));
#5518=CARTESIAN_POINT('Ctrl Pts',(6.4430005297901,-3.7905877946382,-1.20735040930033));
#5519=CARTESIAN_POINT('Ctrl Pts',(6.4430005297901,-3.95787261855977,-0.715467908482556));
#5520=CARTESIAN_POINT('Ctrl Pts',(6.4430005297901,-4.0999785741866,0.321696095215354));
#5521=CARTESIAN_POINT('Ctrl Pts',(6.4430005297901,-4.06691955087291,0.857794436836504));
#5522=CARTESIAN_POINT('Ctrl Pts',(6.4430005297901,-3.79581350913489,1.90493582172488));
#5523=CARTESIAN_POINT('Ctrl Pts',(6.4430005297901,-3.55404702294629,2.40416273654669));
#5524=CARTESIAN_POINT('Ctrl Pts',(6.4430005297901,-2.88474862400959,3.29779955123577));
#5525=CARTESIAN_POINT('Ctrl Pts',(6.4430005297901,-2.45846445810197,3.67959405679302));
#5526=CARTESIAN_POINT('Ctrl Pts',(6.4430005297901,-1.9715811324004,3.97043534620107));
#5527=CARTESIAN_POINT('',(10.4430005297901,-2.16151778945139,-3.03095833168078));
#5528=CARTESIAN_POINT('Ctrl Pts',(10.4430005297901,-2.16151778945139,-3.03095833168078));
#5529=CARTESIAN_POINT('Ctrl Pts',(10.4430005297901,-2.4417969811413,-2.86779155838698));
#5530=CARTESIAN_POINT('Ctrl Pts',(10.4430005297901,-2.69946597133354,-2.66855779259647));
#5531=CARTESIAN_POINT('Ctrl Pts',(10.4430005297901,-3.16313807023027,-2.20413689736136));
#5532=CARTESIAN_POINT('Ctrl Pts',(10.4430005297901,-3.36582061002206,-1.93954623621156));
#5533=CARTESIAN_POINT('Ctrl Pts',(10.4430005297901,-3.7905877946382,-1.20735040930033));
#5534=CARTESIAN_POINT('Ctrl Pts',(10.4430005297901,-3.95787261855977,-0.715467908482556));
#5535=CARTESIAN_POINT('Ctrl Pts',(10.4430005297901,-4.0999785741866,0.321696095215354));
#5536=CARTESIAN_POINT('Ctrl Pts',(10.4430005297901,-4.06691955087291,0.857794436836504));
#5537=CARTESIAN_POINT('Ctrl Pts',(10.4430005297901,-3.79581350913489,1.90493582172488));
#5538=CARTESIAN_POINT('Ctrl Pts',(10.4430005297901,-3.55404702294629,2.40416273654669));
#5539=CARTESIAN_POINT('Ctrl Pts',(10.4430005297901,-2.88474862400959,3.29779955123577));
#5540=CARTESIAN_POINT('Ctrl Pts',(10.4430005297901,-2.45846445810197,3.67959405679302));
#5541=CARTESIAN_POINT('Ctrl Pts',(10.4430005297901,-1.9715811324004,3.97043534620107));
#5542=CARTESIAN_POINT('',(6.4430005297901,-2.16151778945139,-3.03095833168078));
#5543=CARTESIAN_POINT('Origin',(6.4430005297901,-2.77555756156289E-16,5.55111512312578E-16));
#5544=CARTESIAN_POINT('Origin',(6.4430005297901,-2.77555756156289E-16,5.55111512312578E-16));
#5545=CARTESIAN_POINT('Origin',(10.4430005297901,-2.77555756156289E-16,
5.55111512312578E-16));
#5546=CARTESIAN_POINT('Origin',(6.4430005297901,7.33246945257534,-3.33066907387547E-15));
#5547=CARTESIAN_POINT('',(6.4430005297901,7.33246945257534,-3.33066907387547E-15));
#5548=CARTESIAN_POINT('',(6.4430005297901,3.66623472628768,6.35010481840362));
#5549=CARTESIAN_POINT('',(6.4430005297901,7.33246945257534,-3.33066907387547E-15));
#5550=CARTESIAN_POINT('',(10.4430005297901,3.66623472628768,6.35010481840362));
#5551=CARTESIAN_POINT('',(6.4430005297901,3.66623472628768,6.35010481840362));
#5552=CARTESIAN_POINT('',(10.4430005297901,7.33246945257534,-3.33066907387547E-15));
#5553=CARTESIAN_POINT('',(10.4430005297901,7.33246945257534,-3.33066907387547E-15));
#5554=CARTESIAN_POINT('',(6.4430005297901,7.33246945257534,-3.33066907387547E-15));
#5555=CARTESIAN_POINT('Origin',(6.4430005297901,3.66623472628767,-6.35010481840363));
#5556=CARTESIAN_POINT('',(6.4430005297901,3.66623472628767,-6.35010481840363));
#5557=CARTESIAN_POINT('',(6.4430005297901,3.66623472628767,-6.35010481840363));
#5558=CARTESIAN_POINT('',(10.4430005297901,3.66623472628767,-6.35010481840363));
#5559=CARTESIAN_POINT('',(10.4430005297901,3.66623472628767,-6.35010481840363));
#5560=CARTESIAN_POINT('',(6.4430005297901,3.66623472628767,-6.35010481840363));
#5561=CARTESIAN_POINT('Origin',(6.4430005297901,-3.66623472628767,-6.35010481840362));
#5562=CARTESIAN_POINT('',(6.4430005297901,-3.66623472628767,-6.35010481840362));
#5563=CARTESIAN_POINT('',(6.4430005297901,-3.66623472628767,-6.35010481840362));
#5564=CARTESIAN_POINT('',(10.4430005297901,-3.66623472628767,-6.35010481840362));
#5565=CARTESIAN_POINT('',(10.4430005297901,-3.66623472628767,-6.35010481840362));
#5566=CARTESIAN_POINT('',(6.4430005297901,-3.66623472628767,-6.35010481840362));
#5567=CARTESIAN_POINT('Origin',(6.4430005297901,-7.33246945257535,2.77555756156289E-15));
#5568=CARTESIAN_POINT('',(6.4430005297901,-7.33246945257535,2.77555756156289E-15));
#5569=CARTESIAN_POINT('',(6.4430005297901,-7.33246945257535,2.77555756156289E-15));
#5570=CARTESIAN_POINT('',(10.4430005297901,-7.33246945257535,2.77555756156289E-15));
#5571=CARTESIAN_POINT('',(10.4430005297901,-7.33246945257535,2.77555756156289E-15));
#5572=CARTESIAN_POINT('',(6.4430005297901,-7.33246945257535,2.77555756156289E-15));
#5573=CARTESIAN_POINT('Origin',(6.4430005297901,-3.66623472628767,6.35010481840363));
#5574=CARTESIAN_POINT('',(6.4430005297901,-3.66623472628767,6.35010481840363));
#5575=CARTESIAN_POINT('',(6.4430005297901,-3.66623472628767,6.35010481840363));
#5576=CARTESIAN_POINT('',(10.4430005297901,-3.66623472628767,6.35010481840363));
#5577=CARTESIAN_POINT('',(10.4430005297901,-3.66623472628767,6.35010481840363));
#5578=CARTESIAN_POINT('',(6.4430005297901,-3.66623472628767,6.35010481840363));
#5579=CARTESIAN_POINT('Origin',(6.4430005297901,3.66623472628768,6.35010481840362));
#5580=CARTESIAN_POINT('',(6.4430005297901,3.66623472628768,6.35010481840362));
#5581=CARTESIAN_POINT('',(10.4430005297901,3.66623472628768,6.35010481840362));
#5582=CARTESIAN_POINT('Origin',(10.4430005297901,0.,0.));
#5583=CARTESIAN_POINT('Origin',(6.4430005297901,0.,0.));
#5584=CARTESIAN_POINT('',(0.,0.,0.));
#5585=CARTESIAN_POINT('Origin',(3.02384907614375,-2.84862442585767,-2.80808455720391));
#5586=CARTESIAN_POINT('',(11.0238443243108,-2.84860562949496,-1.77825041122887));
#5587=CARTESIAN_POINT('',(10.9314356691441,-2.84862442585767,-1.5071351773836));
#5588=CARTESIAN_POINT('Ctrl Pts',(11.0238395724777,-2.84862442585767,-1.77821291115482));
#5589=CARTESIAN_POINT('Ctrl Pts',(11.023058671384,-2.84862442585767,-1.77602158816867));
#5590=CARTESIAN_POINT('Ctrl Pts',(11.0222784621947,-2.84862442585824,-1.7738300165061));
#5591=CARTESIAN_POINT('Ctrl Pts',(11.0062774820837,-2.84862442585824,-1.72883879945583));
#5592=CARTESIAN_POINT('Ctrl Pts',(10.9913133628153,-2.84862442585851,-1.68592261376175));
#5593=CARTESIAN_POINT('Ctrl Pts',(10.9612482690896,-2.84862442585851,-1.59778423981652));
#5594=CARTESIAN_POINT('Ctrl Pts',(10.9461611622631,-2.84862442585767,-1.55250504487283));
#5595=CARTESIAN_POINT('Ctrl Pts',(10.9314356691441,-2.84862442585767,-1.5071351773836));
#5596=CARTESIAN_POINT('',(11.0238490787776,-2.84862442708621,2.51132611197218));
#5597=CARTESIAN_POINT('',(11.0238490761438,-2.84862442585767,6.75363122348402));
#5598=CARTESIAN_POINT('',(10.7378093816896,-2.84862442585767,1.50713517738359));
#5599=CARTESIAN_POINT('Ctrl Pts',(10.7378093816896,-2.84862442585767,1.5071351773836));
#5600=CARTESIAN_POINT('Ctrl Pts',(10.7745509100274,-2.84862442585767,1.67768015510688));
#5601=CARTESIAN_POINT('Ctrl Pts',(10.8181799183082,-2.84862442695797,1.84746530235002));
#5602=CARTESIAN_POINT('Ctrl Pts',(10.9144539328214,-2.84862442695797,2.18146463191032));
#5603=CARTESIAN_POINT('Ctrl Pts',(10.9675731917165,-2.84862442585767,2.34753476778138));
#5604=CARTESIAN_POINT('Ctrl Pts',(11.0238490840452,-2.84862442585767,2.51132611046758));
#5605=CARTESIAN_POINT('',(10.4912624831434,-2.84862442585767,1.50713517738358));
#5606=CARTESIAN_POINT('',(13.3346225254169,-2.84862442585767,1.50713517738359));
#5607=CARTESIAN_POINT('',(10.0266595508789,-2.8468189348389,2.71028906341842));
#5608=CARTESIAN_POINT('Ctrl Pts',(10.0267941012523,-2.84862442585767,2.70859765771964));
#5609=CARTESIAN_POINT('Ctrl Pts',(10.0337979544476,-2.84862442585767,2.69250499494907));
#5610=CARTESIAN_POINT('Ctrl Pts',(10.0407818720682,-2.84862442585767,2.67640214955592));
#5611=CARTESIAN_POINT('Ctrl Pts',(10.1253566086339,-2.84862442585767,2.48069385236447));
#5612=CARTESIAN_POINT('Ctrl Pts',(10.2012319741895,-2.84862442733188,2.29789169628234));
#5613=CARTESIAN_POINT('Ctrl Pts',(10.3504646709377,-2.84862442733188,1.91583275087761));
#5614=CARTESIAN_POINT('Ctrl Pts',(10.4249778185909,-2.84862442585767,1.7113610340671));
#5615=CARTESIAN_POINT('Ctrl Pts',(10.4912624831434,-2.84862442585767,1.5071351773836));
#5616=CARTESIAN_POINT('',(9.84333250807827,-2.84681996108769,2.71028970167779));
#5617=CARTESIAN_POINT('',(11.0238490761438,-2.84862442585767,2.71179421793157));
#5618=CARTESIAN_POINT('',(9.48780938168963,-2.84862442585767,1.50713517738359));
#5619=CARTESIAN_POINT('Ctrl Pts',(9.48780938168963,-2.84862442585767,1.5071351773836));
#5620=CARTESIAN_POINT('Ctrl Pts',(9.53185899985944,-2.84862442585767,1.71160247880986));
#5621=CARTESIAN_POINT('Ctrl Pts',(9.58587318685495,-2.84862442792121,1.91525078718682));
#5622=CARTESIAN_POINT('Ctrl Pts',(9.70094960223702,-2.84862442792121,2.2980896617317));
#5623=CARTESIAN_POINT('Ctrl Pts',(9.76180678295297,-2.84862442585767,2.48053952383311));
#5624=CARTESIAN_POINT('Ctrl Pts',(9.8318097489011,-2.84862442585767,2.67629614457399));
#5625=CARTESIAN_POINT('Ctrl Pts',(9.83762325462799,-2.84862442585767,2.69245362484614));
#5626=CARTESIAN_POINT('Ctrl Pts',(9.84346698885961,-2.84862442585767,2.70859905909217));
#5627=CARTESIAN_POINT('',(9.24126248314343,-2.84862442585767,1.50713517738358));
#5628=CARTESIAN_POINT('',(13.3346225254169,-2.84862442585767,1.50713517738359));
#5629=CARTESIAN_POINT('',(8.77665954841816,-2.84682622407918,2.71029357769836));
#5630=CARTESIAN_POINT('Ctrl Pts',(8.77679361475528,-2.84862442585767,2.70860756651644));
#5631=CARTESIAN_POINT('Ctrl Pts',(8.78379792777184,-2.84862442585767,2.69251369706502));
#5632=CARTESIAN_POINT('Ctrl Pts',(8.79078230243175,-2.84862442585767,2.67640964375849));
#5633=CARTESIAN_POINT('Ctrl Pts',(8.8753576224118,-2.84862442585767,2.48069807460854));
#5634=CARTESIAN_POINT('Ctrl Pts',(8.95123295617157,-2.8486244273253,2.29789414186475));
#5635=CARTESIAN_POINT('Ctrl Pts',(9.10046525102538,-2.8486244273253,1.91583271764201));
#5636=CARTESIAN_POINT('Ctrl Pts',(9.17497777181831,-2.84862442585767,1.71136117817557));
#5637=CARTESIAN_POINT('Ctrl Pts',(9.24126248314343,-2.84862442585767,1.50713517738359));
#5638=CARTESIAN_POINT('',(8.59333250457579,-2.84682735336114,2.71029427328404));
#5639=CARTESIAN_POINT('',(11.0238490761438,-2.84862442585767,2.71179421793157));
#5640=CARTESIAN_POINT('',(8.23780938168963,-2.84862442585767,1.50713517738359));
#5641=CARTESIAN_POINT('Ctrl Pts',(8.23780938168964,-2.84862442585767,1.5071351773836));
#5642=CARTESIAN_POINT('Ctrl Pts',(8.28185902228173,-2.84862442585767,1.7116025828885));
#5643=CARTESIAN_POINT('Ctrl Pts',(8.33587259560373,-2.84862442791195,1.91525079323359));
#5644=CARTESIAN_POINT('Ctrl Pts',(8.45094825529517,-2.84862442791195,2.29809205765932));
#5645=CARTESIAN_POINT('Ctrl Pts',(8.51180523038482,-2.84862442585767,2.48054376287594));
#5646=CARTESIAN_POINT('Ctrl Pts',(8.58180849741605,-2.84862442585767,2.67630369365445));
#5647=CARTESIAN_POINT('Ctrl Pts',(8.58762237980882,-2.84862442585767,2.69246241698621));
#5648=CARTESIAN_POINT('Ctrl Pts',(8.59346649505355,-2.84862442585767,2.70860909277272));
#5649=CARTESIAN_POINT('',(7.99126248314343,-2.84862442585767,1.50713517738358));
#5650=CARTESIAN_POINT('',(13.3346225254169,-2.84862442585767,1.50713517738359));
#5651=CARTESIAN_POINT('',(7.52665953824353,-2.84683426299416,2.71029850764342));
#5652=CARTESIAN_POINT('Ctrl Pts',(7.52679307496196,-2.84862442585767,2.70861838061488));
#5653=CARTESIAN_POINT('Ctrl Pts',(7.53379789201695,-2.84862442585767,2.6925231903734));
#5654=CARTESIAN_POINT('Ctrl Pts',(7.54078276765018,-2.84862442585767,2.67641781492382));
#5655=CARTESIAN_POINT('Ctrl Pts',(7.62535873067299,-2.84862442585767,2.48070267374547));
#5656=CARTESIAN_POINT('Ctrl Pts',(7.70123402906389,-2.84862442731812,2.29789681034083));
#5657=CARTESIAN_POINT('Ctrl Pts',(7.85046588841197,-2.84862442731812,1.91583267628874));
#5658=CARTESIAN_POINT('Ctrl Pts',(7.92497771912674,-2.84862442585767,1.7113613405205));
#5659=CARTESIAN_POINT('Ctrl Pts',(7.99126248314342,-2.84862442585767,1.5071351773836));
#5660=CARTESIAN_POINT('',(7.34333249310138,-2.84683551217853,2.71029926941601));
#5661=CARTESIAN_POINT('',(11.0238490761438,-2.84862442585767,2.71179421793157));
#5662=CARTESIAN_POINT('',(6.98780938168963,-2.84862442585767,1.50713517738359));
#5663=CARTESIAN_POINT('Ctrl Pts',(6.98780938168963,-2.84862442585767,1.5071351773836));
#5664=CARTESIAN_POINT('Ctrl Pts',(7.0318590477534,-2.84862442585767,1.71160270112162));
#5665=CARTESIAN_POINT('Ctrl Pts',(7.08587194364161,-2.84862442790181,1.91525079631235));
#5666=CARTESIAN_POINT('Ctrl Pts',(7.20094677397292,-2.84862442790181,2.29809467489166));
#5667=CARTESIAN_POINT('Ctrl Pts',(7.26180352074679,-2.84862442585766,2.48054838492829));
#5668=CARTESIAN_POINT('Ctrl Pts',(7.33180711870137,-2.84862442585766,2.67631193139019));
#5669=CARTESIAN_POINT('Ctrl Pts',(7.33762141389105,-2.84862442585767,2.69247201579432));
#5670=CARTESIAN_POINT('Ctrl Pts',(7.34346594671238,-2.84862442585767,2.70862005097966));
#5671=CARTESIAN_POINT('',(6.74126248314343,-2.84862442585767,1.50713517738358));
#5672=CARTESIAN_POINT('',(13.3346225254169,-2.84862442585767,1.50713517738359));
#5673=CARTESIAN_POINT('',(6.27665951841218,-2.8468431775105,2.71030391927814));
#5674=CARTESIAN_POINT('Ctrl Pts',(6.27679247260682,-2.84862442585767,2.70863024324506));
#5675=CARTESIAN_POINT('Ctrl Pts',(6.28379784512061,-2.84862442585767,2.69253359968691));
#5676=CARTESIAN_POINT('Ctrl Pts',(6.29078327281752,-2.84862442585768,2.67642676942568));
#5677=CARTESIAN_POINT('Ctrl Pts',(6.37535994854178,-2.84862442585768,2.48070770856496));
#5678=CARTESIAN_POINT('Ctrl Pts',(6.45123520736229,-2.84862442731026,2.29789973691976));
#5679=CARTESIAN_POINT('Ctrl Pts',(6.60046659256744,-2.84862442731026,1.91583262505285));
#5680=CARTESIAN_POINT('Ctrl Pts',(6.67497765942542,-2.84862442585767,1.71136152446282));
#5681=CARTESIAN_POINT('Ctrl Pts',(6.74126248314343,-2.84862442585767,1.50713517738359));
#5682=CARTESIAN_POINT('',(6.09333247164065,-2.84684456741434,2.71030475812859));
#5683=CARTESIAN_POINT('',(11.0238490761438,-2.84862442585767,2.71179421793157));
#5684=CARTESIAN_POINT('',(5.73780938168963,-2.84862442585767,1.50713517738359));
#5685=CARTESIAN_POINT('Ctrl Pts',(5.73780938168963,-2.84862442585767,1.5071351773836));
#5686=CARTESIAN_POINT('Ctrl Pts',(5.78185907685439,-2.84862442585767,1.71160283620116));
#5687=CARTESIAN_POINT('Ctrl Pts',(5.83587122068751,-2.84862442789063,1.91525079561866));
#5688=CARTESIAN_POINT('Ctrl Pts',(5.9509451358443,-2.84862442789063,2.29809754881907));
#5689=CARTESIAN_POINT('Ctrl Pts',(6.01180162763585,-2.84862442585767,2.48055345043311));
#5690=CARTESIAN_POINT('Ctrl Pts',(6.08180559131495,-2.84862442585767,2.67632096708642));
#5691=CARTESIAN_POINT('Ctrl Pts',(6.08762034133423,-2.84862442585767,2.69248254974333));
#5692=CARTESIAN_POINT('Ctrl Pts',(6.09346533427394,-2.84862442585767,2.70863208133986));
#5693=CARTESIAN_POINT('',(5.49126248314343,-2.84862442585767,1.50713517738358));
#5694=CARTESIAN_POINT('',(13.3346225254169,-2.84862442585767,1.50713517738359));
#5695=CARTESIAN_POINT('',(5.02665948642913,-2.846853123834,2.71030989419903));
#5696=CARTESIAN_POINT('Ctrl Pts',(5.02679179614449,-2.84862442585767,2.70864333135427));
#5697=CARTESIAN_POINT('Ctrl Pts',(5.03379778445795,-2.84862442585767,2.69254507916332));
#5698=CARTESIAN_POINT('Ctrl Pts',(5.04078382417434,-2.84862442585766,2.67643663859843));
#5699=CARTESIAN_POINT('Ctrl Pts',(5.12536129472081,-2.84862442585766,2.48071325160255));
#5700=CARTESIAN_POINT('Ctrl Pts',(5.20123650898541,-2.84862442730161,2.29790296509866));
#5701=CARTESIAN_POINT('Ctrl Pts',(5.35046737523669,-2.84862442730161,1.91583256170217));
#5702=CARTESIAN_POINT('Ctrl Pts',(5.42497759134768,-2.84862442585767,1.7113617342132));
#5703=CARTESIAN_POINT('Ctrl Pts',(5.49126248314342,-2.84862442585767,1.5071351773836));
#5704=CARTESIAN_POINT('',(4.84333243760253,-2.84685468045443,2.71031082368254));
#5705=CARTESIAN_POINT('',(11.0238490761438,-2.84862442585767,2.71179421793157));
#5706=CARTESIAN_POINT('',(4.48780938168963,-2.84862442585767,1.50713517738359));
#5707=CARTESIAN_POINT('Ctrl Pts',(4.48780938168963,-2.84862442585767,1.5071351773836));
#5708=CARTESIAN_POINT('Ctrl Pts',(4.53185911031318,-2.84862442585767,1.71160299150844));
#5709=CARTESIAN_POINT('Ctrl Pts',(4.58587041394647,-2.84862442787828,1.9152507901144));
#5710=CARTESIAN_POINT('Ctrl Pts',(4.70094331303715,-2.84862442787828,2.29810072324551));
#5711=CARTESIAN_POINT('Ctrl Pts',(4.76179951821517,-2.84862442585766,2.48055903410995));
#5712=CARTESIAN_POINT('Ctrl Pts',(4.83180388858748,-2.84862442585766,2.67633093595801));
#5713=CARTESIAN_POINT('Ctrl Pts',(4.83761914279346,-2.84862442585767,2.69249417782208));
#5714=CARTESIAN_POINT('Ctrl Pts',(4.84346464580177,-2.84862442585767,2.70864536656847));
#5715=CARTESIAN_POINT('',(4.24126248314343,-2.84862442585767,1.50713517738358));
#5716=CARTESIAN_POINT('',(13.3346225254169,-2.84862442585767,1.50713517738359));
#5717=CARTESIAN_POINT('',(3.77665943905189,-2.84686429817697,2.71031653458594));
#5718=CARTESIAN_POINT('Ctrl Pts',(3.77679103100252,-2.84862442585767,2.70865786644558));
#5719=CARTESIAN_POINT('Ctrl Pts',(3.78379770666065,-2.84862442585767,2.69255782170753));
#5720=CARTESIAN_POINT('Ctrl Pts',(3.7907844294769,-2.84862442585767,2.6764475867298));
#5721=CARTESIAN_POINT('Ctrl Pts',(3.87536279264918,-2.84862442585767,2.48071939353203));
#5722=CARTESIAN_POINT('Ctrl Pts',(3.95123795638205,-2.84862442729201,2.29790654931287));
#5723=CARTESIAN_POINT('Ctrl Pts',(4.10046825118152,-2.84862442729201,1.91583248336832));
#5724=CARTESIAN_POINT('Ctrl Pts',(4.17497751316149,-2.84862442585767,1.71136197510816));
#5725=CARTESIAN_POINT('Ctrl Pts',(4.24126248314342,-2.84862442585767,1.5071351773836));
#5726=CARTESIAN_POINT('',(3.59371978829928,-2.84790817158154,2.71073122597795));
#5727=CARTESIAN_POINT('',(11.0238490761438,-2.84862442585767,2.71179421793157));
#5728=CARTESIAN_POINT('',(3.23780938168963,-2.84862442585767,1.50713517738359));
#5729=CARTESIAN_POINT('Ctrl Pts',(3.23780938168963,-2.84862442585767,1.50713517738361));
#5730=CARTESIAN_POINT('Ctrl Pts',(3.28186054745108,-2.84862442585767,1.71160966234283));
#5731=CARTESIAN_POINT('Ctrl Pts',(3.33582269739854,-2.84862442724084,1.91524933773065));
#5732=CARTESIAN_POINT('Ctrl Pts',(3.45073483075678,-2.84862442724084,2.2979205346272));
#5733=CARTESIAN_POINT('Ctrl Pts',(3.51144589960124,-2.84862442585768,2.48014616288996));
#5734=CARTESIAN_POINT('Ctrl Pts',(3.58146712224872,-2.84862442585768,2.67616260726964));
#5735=CARTESIAN_POINT('Ctrl Pts',(3.58743530933706,-2.84862442585767,2.69276463740784));
#5736=CARTESIAN_POINT('Ctrl Pts',(3.59343543922426,-2.84862442585767,2.70935393890616));
#5737=CARTESIAN_POINT('',(3.02384907614375,-2.84862442585767,1.50713517738359));
#5738=CARTESIAN_POINT('',(13.3346225254169,-2.84862442585767,1.50713517738359));
#5739=CARTESIAN_POINT('',(3.02384907614375,-2.84819869582995,-2.12547276695727));
#5740=CARTESIAN_POINT('',(3.02384907614375,-2.84862442585767,-1.40404227860195));
#5741=CARTESIAN_POINT('',(3.18488877059788,-2.84862442585766,-1.50713517738361));
#5742=CARTESIAN_POINT('Ctrl Pts',(3.18488877059788,-2.84862442585767,-1.50713517738361));
#5743=CARTESIAN_POINT('Ctrl Pts',(3.16242044753531,-2.84862442585767,-1.61142750896447));
#5744=CARTESIAN_POINT('Ctrl Pts',(3.137405991007,-2.84862442595863,-1.71531300796113));
#5745=CARTESIAN_POINT('Ctrl Pts',(3.0834656597595,-2.84862442595863,-1.92105514468293));
#5746=CARTESIAN_POINT('Ctrl Pts',(3.0544704326137,-2.84862442585767,-2.02327555320667));
#5747=CARTESIAN_POINT('Ctrl Pts',(3.02384907614375,-2.84862442585767,-2.12477398354848));
#5748=CARTESIAN_POINT('',(3.43143566914408,-2.84862442585766,-1.5071351773836));
#5749=CARTESIAN_POINT('',(13.3346225254169,-2.84862442585767,-1.50713517738359));
#5750=CARTESIAN_POINT('',(3.89603869449459,-2.84686019521323,-2.71031410479823));
#5751=CARTESIAN_POINT('Ctrl Pts',(3.89590683973102,-2.84862442585767,-2.70865254916596));
#5752=CARTESIAN_POINT('Ctrl Pts',(3.88889722083,-2.84862442585767,-2.69254581918906));
#5753=CARTESIAN_POINT('Ctrl Pts',(3.88190757115915,-2.84862442585768,-2.67642888977708));
#5754=CARTESIAN_POINT('Ctrl Pts',(3.79732623229834,-2.84862442585768,-2.48069416593426));
#5755=CARTESIAN_POINT('Ctrl Pts',(3.7214509531498,-2.84862442738219,-2.29788126150319));
#5756=CARTESIAN_POINT('Ctrl Pts',(3.57222405172544,-2.84862442738219,-1.91581557178352));
#5757=CARTESIAN_POINT('Ctrl Pts',(3.49771788311829,-2.84862442585767,-1.71135348373173));
#5758=CARTESIAN_POINT('Ctrl Pts',(3.43143566914408,-2.84862442585767,-1.50713517738359));
#5759=CARTESIAN_POINT('',(4.07936573032278,-2.84685854325951,-2.71031312383777));
#5760=CARTESIAN_POINT('',(11.0238490761438,-2.84862442585767,-2.71179421793157));
#5761=CARTESIAN_POINT('',(4.43488877059788,-2.84862442585766,-1.50713517738361));
#5762=CARTESIAN_POINT('Ctrl Pts',(4.43488877059788,-2.84862442585767,-1.50713517738361));
#5763=CARTESIAN_POINT('Ctrl Pts',(4.39082934716643,-2.84862442585767,-1.71164799237998));
#5764=CARTESIAN_POINT('Ctrl Pts',(4.33680421314192,-2.84862442782486,-1.91534068114032));
#5765=CARTESIAN_POINT('Ctrl Pts',(4.22171428517076,-2.84862442782486,-2.29822947317743));
#5766=CARTESIAN_POINT('Ctrl Pts',(4.16085761026589,-2.84862442585767,-2.48068346557449));
#5767=CARTESIAN_POINT('Ctrl Pts',(4.09086679229697,-2.84862442585767,-2.67641287300669));
#5768=CARTESIAN_POINT('Ctrl Pts',(4.08506533437374,-2.84862442585767,-2.69253763418667));
#5769=CARTESIAN_POINT('Ctrl Pts',(4.07923377064371,-2.84862442585767,-2.70865040206242));
#5770=CARTESIAN_POINT('',(4.68143566914408,-2.84862442585766,-1.5071351773836));
#5771=CARTESIAN_POINT('',(13.3346225254169,-2.84862442585767,-1.50713517738359));
#5772=CARTESIAN_POINT('',(5.1460386529845,-2.84684948021485,-2.71030771277531));
#5773=CARTESIAN_POINT('Ctrl Pts',(5.14590610781719,-2.84862442585767,-2.70863855402169));
#5774=CARTESIAN_POINT('Ctrl Pts',(5.13889714963154,-2.84862442585767,-2.69253354823215));
#5775=CARTESIAN_POINT('Ctrl Pts',(5.13190815660042,-2.84862442585766,-2.67641834479668));
#5776=CARTESIAN_POINT('Ctrl Pts',(5.04732767386717,-2.84862442585766,-2.48068824836471));
#5777=CARTESIAN_POINT('Ctrl Pts',(4.97145234642707,-2.8486244273917,-2.29787781119133));
#5778=CARTESIAN_POINT('Ctrl Pts',(4.82222489298551,-2.8486244273917,-1.91581564514287));
#5779=CARTESIAN_POINT('Ctrl Pts',(4.74771780885373,-2.84862442585767,-1.71135325491949));
#5780=CARTESIAN_POINT('Ctrl Pts',(4.68143566914408,-2.84862442585767,-1.50713517738359));
#5781=CARTESIAN_POINT('',(5.32936569108213,-2.84684801042969,-2.71030683048953));
#5782=CARTESIAN_POINT('',(11.0238490761438,-2.84862442585767,-2.71179421793157));
#5783=CARTESIAN_POINT('',(5.68488877059788,-2.84862442585766,-1.50713517738361));
#5784=CARTESIAN_POINT('Ctrl Pts',(5.68488877059787,-2.84862442585767,-1.50713517738361));
#5785=CARTESIAN_POINT('Ctrl Pts',(5.64082938247698,-2.84862442585767,-1.71164782847729));
#5786=CARTESIAN_POINT('Ctrl Pts',(5.58680337295899,-2.84862442783755,-1.91534068797091));
#5787=CARTESIAN_POINT('Ctrl Pts',(5.47171238880716,-2.84862442783755,-2.29822617883969));
#5788=CARTESIAN_POINT('Ctrl Pts',(5.41085541472201,-2.84862442585768,-2.48067767630624));
#5789=CARTESIAN_POINT('Ctrl Pts',(5.34086501982091,-2.84862442585768,-2.67640253517119));
#5790=CARTESIAN_POINT('Ctrl Pts',(5.335064085706,-2.84862442585767,-2.69252557390748));
#5791=CARTESIAN_POINT('Ctrl Pts',(5.32923305188914,-2.84862442585767,-2.70863662146847));
#5792=CARTESIAN_POINT('',(5.93143566914408,-2.84862442585766,-1.5071351773836));
#5793=CARTESIAN_POINT('',(13.3346225254169,-2.84862442585767,-1.50713517738359));
#5794=CARTESIAN_POINT('',(6.39603862562206,-2.8468399185786,-2.7103019473717));
#5795=CARTESIAN_POINT('Ctrl Pts',(6.39590545902977,-2.84862442585767,-2.70862592165797));
#5796=CARTESIAN_POINT('Ctrl Pts',(6.38889709426525,-2.84862442585767,-2.69252246698333));
#5797=CARTESIAN_POINT('Ctrl Pts',(6.381908691017,-2.84862442585767,-2.67640881627049));
#5798=CARTESIAN_POINT('Ctrl Pts',(6.29732897257062,-2.84862442585767,-2.48068289513417));
#5799=CARTESIAN_POINT('Ctrl Pts',(6.22145360243729,-2.8486244274003,-2.29787469612044));
#5800=CARTESIAN_POINT('Ctrl Pts',(6.07222564657022,-2.8486244274003,-1.91581570455012));
#5801=CARTESIAN_POINT('Ctrl Pts',(5.99771774402429,-2.84862442585767,-1.71135305517723));
#5802=CARTESIAN_POINT('Ctrl Pts',(5.93143566914408,-2.84862442585767,-1.50713517738359));
#5803=CARTESIAN_POINT('',(6.57936566550857,-2.84683860176748,-2.71030114855983));
#5804=CARTESIAN_POINT('',(11.0238490761438,-2.84862442585767,-2.71179421793157));
#5805=CARTESIAN_POINT('',(6.93488877059788,-2.84862442585766,-1.50713517738361));
#5806=CARTESIAN_POINT('Ctrl Pts',(6.93488877059789,-2.84862442585767,-1.5071351773836));
#5807=CARTESIAN_POINT('Ctrl Pts',(6.89082941311706,-2.84862442585767,-1.71164768625373));
#5808=CARTESIAN_POINT('Ctrl Pts',(6.83680262185114,-2.84862442784899,-1.91534068961923));
#5809=CARTESIAN_POINT('Ctrl Pts',(6.72171068862222,-2.84862442784899,-2.29822320309697));
#5810=CARTESIAN_POINT('Ctrl Pts',(6.66085344903225,-2.84862442585767,-2.48067243596248));
#5811=CARTESIAN_POINT('Ctrl Pts',(6.59086343368136,-2.84862442585767,-2.67639318603298));
#5812=CARTESIAN_POINT('Ctrl Pts',(6.58506297100052,-2.84862442585767,-2.69251467300301));
#5813=CARTESIAN_POINT('Ctrl Pts',(6.5792324140922,-2.84862442585767,-2.70862417070381));
#5814=CARTESIAN_POINT('',(7.18143566914408,-2.84862442585767,-1.5071351773836));
#5815=CARTESIAN_POINT('',(13.3346225254169,-2.84862442585767,-1.50713517738359));
#5816=CARTESIAN_POINT('',(7.64603860945592,-2.84683132955625,-2.71029671436601));
#5817=CARTESIAN_POINT('Ctrl Pts',(7.64590487996825,-2.84862442585767,-2.70861444779753));
#5818=CARTESIAN_POINT('Ctrl Pts',(7.63889705165458,-2.84862442585767,-2.69251239752542));
#5819=CARTESIAN_POINT('Ctrl Pts',(7.63190918158326,-2.84862442585767,-2.67640015265958));
#5820=CARTESIAN_POINT('Ctrl Pts',(7.54733015001958,-2.84862442585767,-2.48067802259182));
#5821=CARTESIAN_POINT('Ctrl Pts',(7.47145474188106,-2.84862442740813,-2.29787186609686));
#5822=CARTESIAN_POINT('Ctrl Pts',(7.3222263260763,-2.84862442740813,-1.91581575263515));
#5823=CARTESIAN_POINT('Ctrl Pts',(7.2477176870411,-2.84862442585767,-1.7113528796096));
#5824=CARTESIAN_POINT('Ctrl Pts',(7.18143566914408,-2.84862442585767,-1.50713517738359));
#5825=CARTESIAN_POINT('',(7.8293656507619,-2.84683014249272,-2.71029598689785));
#5826=CARTESIAN_POINT('',(11.0238490761438,-2.84862442585767,-2.71179421793157));
#5827=CARTESIAN_POINT('',(8.18488877059788,-2.84862442585766,-1.50713517738361));
#5828=CARTESIAN_POINT('Ctrl Pts',(8.18488877059787,-2.84862442585767,-1.50713517738361));
#5829=CARTESIAN_POINT('Ctrl Pts',(8.14082943988044,-2.84862442585767,-1.71164756202476));
#5830=CARTESIAN_POINT('Ctrl Pts',(8.08680194594983,-2.84862442785935,-1.91534068721287));
#5831=CARTESIAN_POINT('Ctrl Pts',(7.97170915442048,-2.84862442785935,-2.29822049854839));
#5832=CARTESIAN_POINT('Ctrl Pts',(7.910851677616,-2.84862442585767,-2.48066766373789));
#5833=CARTESIAN_POINT('Ctrl Pts',(7.84086200497834,-2.84862442585767,-2.67638467936083));
#5834=CARTESIAN_POINT('Ctrl Pts',(7.83506196928568,-2.84862442585767,-2.69250475952157));
#5835=CARTESIAN_POINT('Ctrl Pts',(7.82923184430401,-2.84862442585767,-2.70861285213785));
#5836=CARTESIAN_POINT('',(8.43143566914408,-2.84862442585767,-1.5071351773836));
#5837=CARTESIAN_POINT('',(13.3346225254169,-2.84862442585767,-1.50713517738359));
#5838=CARTESIAN_POINT('',(8.89603860220502,-2.84682356859058,-2.71029193815233));
#5839=CARTESIAN_POINT('Ctrl Pts',(8.89590435996554,-2.84862442585767,-2.70860396846321));
#5840=CARTESIAN_POINT('Ctrl Pts',(8.88889701939368,-2.84862442585767,-2.69250319699323));
#5841=CARTESIAN_POINT('Ctrl Pts',(8.881909634102,-2.84862442585767,-2.67639223223817));
#5842=CARTESIAN_POINT('Ctrl Pts',(8.79733122354344,-2.84862442585767,-2.48067356350021));
#5843=CARTESIAN_POINT('Ctrl Pts',(8.72145578136366,-2.84862442741529,-2.29786928082383));
#5844=CARTESIAN_POINT('Ctrl Pts',(8.57222694237506,-2.84862442741529,-1.91581579145778));
#5845=CARTESIAN_POINT('Ctrl Pts',(8.49771763664538,-2.84862442585767,-1.71135272433826));
#5846=CARTESIAN_POINT('Ctrl Pts',(8.43143566914408,-2.84862442585767,-1.50713517738359));
#5847=CARTESIAN_POINT('',(9.07936564464315,-2.84682249256182,-2.71029127221896));
#5848=CARTESIAN_POINT('',(11.0238490761438,-2.84862442585767,-2.71179421793157));
#5849=CARTESIAN_POINT('',(9.43488877059788,-2.84862442585766,-1.5071351773836));
#5850=CARTESIAN_POINT('Ctrl Pts',(9.43488877059788,-2.84862442585767,-1.50713517738359));
#5851=CARTESIAN_POINT('Ctrl Pts',(9.39082946339622,-2.84862442585767,-1.71164745287044));
#5852=CARTESIAN_POINT('Ctrl Pts',(9.33680133416077,-2.8486244278688,-1.91534068162397));
#5853=CARTESIAN_POINT('Ctrl Pts',(9.2217077620153,-2.8486244278688,-2.29821802707406));
#5854=CARTESIAN_POINT('Ctrl Pts',(9.16085007199191,-2.84862442585767,-2.48066329456691));
#5855=CARTESIAN_POINT('Ctrl Pts',(9.09086071058218,-2.84862442585767,-2.67637689747843));
#5856=CARTESIAN_POINT('Ctrl Pts',(9.08506106379369,-2.84862442585767,-2.69249569513711));
#5857=CARTESIAN_POINT('Ctrl Pts',(9.07923133219744,-2.84862442585767,-2.70860250681946));
#5858=CARTESIAN_POINT('',(9.68143566914408,-2.84862442585767,-1.5071351773836));
#5859=CARTESIAN_POINT('',(13.3346225254169,-2.84862442585767,-1.50713517738359));
#5860=CARTESIAN_POINT('',(10.1460386020864,-2.8468165186648,-2.71028755728909));
#5861=CARTESIAN_POINT('Ctrl Pts',(10.1459038904249,-2.84862442585767,-2.70859435034995));
#5862=CARTESIAN_POINT('Ctrl Pts',(10.1388969955833,-2.84862442585767,-2.69249474921214));
#5863=CARTESIAN_POINT('Ctrl Pts',(10.1319100533288,-2.84862442585767,-2.67638495598403));
#5864=CARTESIAN_POINT('Ctrl Pts',(10.0473322072149,-2.84862442585767,-2.48066946312399));
#5865=CARTESIAN_POINT('Ctrl Pts',(9.97145673437474,-2.84862442742187,-2.29786690753779));
#5866=CARTESIAN_POINT('Ctrl Pts',(9.82222750426836,-2.84862442742187,-1.91581582264984));
#5867=CARTESIAN_POINT('Ctrl Pts',(9.74771759182774,-2.84862442585767,-1.71135258625323));
#5868=CARTESIAN_POINT('Ctrl Pts',(9.68143566914409,-2.84862442585767,-1.50713517738361));
#5869=CARTESIAN_POINT('',(10.3289257514711,-2.84771184870989,-2.71054614509517));
#5870=CARTESIAN_POINT('',(11.0238490761438,-2.84862442585767,-2.71179421793157));
#5871=CARTESIAN_POINT('',(10.6848887705979,-2.84862442585766,-1.5071351773836));
#5872=CARTESIAN_POINT('Ctrl Pts',(10.6848887705979,-2.84862442585767,-1.50713517738359));
#5873=CARTESIAN_POINT('Ctrl Pts',(10.6408288271577,-2.84862442585767,-1.71165040613047));
#5874=CARTESIAN_POINT('Ctrl Pts',(10.586823565171,-2.84862442755607,-1.9153402145107));
#5875=CARTESIAN_POINT('Ctrl Pts',(10.4718028413942,-2.84862442755607,-2.29814280868909));
#5876=CARTESIAN_POINT('Ctrl Pts',(10.4110099703332,-2.84862442585767,-2.48048848453579));
#5877=CARTESIAN_POINT('Ctrl Pts',(10.3410124389629,-2.84862442585767,-2.67631715615895));
#5878=CARTESIAN_POINT('Ctrl Pts',(10.3351441403831,-2.84862442585767,-2.69263311564845));
#5879=CARTESIAN_POINT('Ctrl Pts',(10.3292450042586,-2.84862442585767,-2.70893678933792));
#5880=CARTESIAN_POINT('',(13.3346225254169,-2.84862442585767,-1.50713517738359));
#5881=CARTESIAN_POINT('Origin',(3.02384907614375,2.84862442585767,2.80808455720391));
#5882=CARTESIAN_POINT('',(10.6511778487968,2.84808967359283,-2.71093915478704));
#5883=CARTESIAN_POINT('',(11.0238490761438,2.84862442585767,-1.77841863815956));
#5884=CARTESIAN_POINT('Ctrl Pts',(10.6517444165533,2.84862442585767,-2.70958663119422));
#5885=CARTESIAN_POINT('Ctrl Pts',(10.7181155081048,2.84862442585767,-2.5572180519126));
#5886=CARTESIAN_POINT('Ctrl Pts',(10.7831857927431,2.84862442636543,-2.40277143381646));
#5887=CARTESIAN_POINT('Ctrl Pts',(10.9075012055968,2.84862442636543,-2.09344139364087));
#5888=CARTESIAN_POINT('Ctrl Pts',(10.9677673094432,2.84862442585767,-1.93595017012862));
#5889=CARTESIAN_POINT('Ctrl Pts',(11.0238490761437,2.84862442585767,-1.77841863815954));
#5890=CARTESIAN_POINT('',(10.4683325073484,2.84681651858225,-2.71028755728349));
#5891=CARTESIAN_POINT('',(11.0238490761438,2.84862442585767,-2.71179421793157));
#5892=CARTESIAN_POINT('',(10.1128093816896,2.84862442585767,-1.50713517738358));
#5893=CARTESIAN_POINT('Ctrl Pts',(10.1128093816896,2.84862442585767,-1.50713517738361));
#5894=CARTESIAN_POINT('Ctrl Pts',(10.1568589896422,2.84862442585767,-1.71160243138402));
#5895=CARTESIAN_POINT('Ctrl Pts',(10.2108734623886,2.84862442792555,-1.91525078325235));
#5896=CARTESIAN_POINT('Ctrl Pts',(10.3259502311565,2.84862442792555,-2.29808853750365));
#5897=CARTESIAN_POINT('Ctrl Pts',(10.3868075072088,2.84862442585767,-2.48053753211887));
#5898=CARTESIAN_POINT('Ctrl Pts',(10.4568103325124,2.84862442585767,-2.6762925996824));
#5899=CARTESIAN_POINT('Ctrl Pts',(10.4626236619148,2.84862442585767,-2.69244949767383));
#5900=CARTESIAN_POINT('Ctrl Pts',(10.4684672177927,2.84862442585767,-2.70859435034994));
#5901=CARTESIAN_POINT('',(9.86626248314343,2.84862442585767,-1.50713517738359));
#5902=CARTESIAN_POINT('',(13.3346225254169,2.84862442585767,-1.50713517738359));
#5903=CARTESIAN_POINT('',(9.40165955050884,2.84682249264362,-2.71029127222451));
#5904=CARTESIAN_POINT('Ctrl Pts',(9.40179386416001,2.84862442585767,-2.70860250681946));
#5905=CARTESIAN_POINT('Ctrl Pts',(9.40879794213361,2.84862442585767,-2.69250925396209));
#5906=CARTESIAN_POINT('Ctrl Pts',(9.41578208317429,2.84862442585767,-2.67640581787988));
#5907=CARTESIAN_POINT('Ctrl Pts',(9.50035710454219,2.84862442585767,-2.48069591960582));
#5908=CARTESIAN_POINT('Ctrl Pts',(9.57623245461227,2.84862442732866,-2.29789289314525));
#5909=CARTESIAN_POINT('Ctrl Pts',(9.72546495433774,2.84862442732866,-1.91583273517924));
#5910=CARTESIAN_POINT('Ctrl Pts',(9.79997779588513,2.84862442585767,-1.71136110402466));
#5911=CARTESIAN_POINT('Ctrl Pts',(9.86626248314343,2.84862442585767,-1.50713517738359));
#5912=CARTESIAN_POINT('',(9.21833250721586,2.84682356850894,-2.71029193814678));
#5913=CARTESIAN_POINT('',(11.0238490761438,2.84862442585767,-2.71179421793157));
#5914=CARTESIAN_POINT('',(8.86280938168963,2.84862442585767,-1.50713517738358));
#5915=CARTESIAN_POINT('Ctrl Pts',(8.86280938168963,2.84862442585767,-1.5071351773836));
#5916=CARTESIAN_POINT('Ctrl Pts',(8.90685901072075,2.84862442585767,-1.71160252922533));
#5917=CARTESIAN_POINT('Ctrl Pts',(8.96087289825601,2.84862442791668,-1.91525079053687));
#5918=CARTESIAN_POINT('Ctrl Pts',(9.07594894433648,2.84862442791668,-2.29809083397137));
#5919=CARTESIAN_POINT('Ctrl Pts',(9.13680602485858,2.84862442585767,-2.48054159879405));
#5920=CARTESIAN_POINT('Ctrl Pts',(9.20680913788998,2.84862442585767,-2.67629983902876));
#5921=CARTESIAN_POINT('Ctrl Pts',(9.21262282775703,2.84862442585767,-2.69245792713028));
#5922=CARTESIAN_POINT('Ctrl Pts',(9.21846674825203,2.84862442585767,-2.70860396846321));
#5923=CARTESIAN_POINT('',(8.61626248314343,2.84862442585767,-1.50713517738359));
#5924=CARTESIAN_POINT('',(13.3346225254169,2.84862442585767,-1.50713517738359));
#5925=CARTESIAN_POINT('',(8.15165954440541,2.84683014257353,-2.71029598690336));
#5926=CARTESIAN_POINT('Ctrl Pts',(8.15179335205343,2.84862442585767,-2.70861285213785));
#5927=CARTESIAN_POINT('Ctrl Pts',(8.15879791114812,2.84862442585767,-2.69251833761412));
#5928=CARTESIAN_POINT('Ctrl Pts',(8.16578253039036,2.84862442585767,-2.67641363857816));
#5929=CARTESIAN_POINT('Ctrl Pts',(8.25035816386072,2.84862442585767,-2.48070032366843));
#5930=CARTESIAN_POINT('Ctrl Pts',(8.32623348041883,2.84862442732179,-2.29789544620645));
#5931=CARTESIAN_POINT('Ctrl Pts',(8.47546556201146,2.84862442732179,-1.91583269807888));
#5932=CARTESIAN_POINT('Ctrl Pts',(8.54997774627531,2.84862442585767,-1.71136125687463));
#5933=CARTESIAN_POINT('Ctrl Pts',(8.61626248314343,2.84862442585767,-1.50713517738358));
#5934=CARTESIAN_POINT('',(7.9683324999494,2.84683132947567,-2.71029671436051));
#5935=CARTESIAN_POINT('',(11.0238490761438,2.84862442585767,-2.71179421793157));
#5936=CARTESIAN_POINT('',(7.61280938168963,2.84862442585767,-1.50713517738358));
#5937=CARTESIAN_POINT('Ctrl Pts',(7.61280938168963,2.84862442585767,-1.5071351773836));
#5938=CARTESIAN_POINT('Ctrl Pts',(7.65685903460308,2.84862442585767,-1.71160264008112));
#5939=CARTESIAN_POINT('Ctrl Pts',(7.71087227780285,2.84862442790699,-1.91525079518883));
#5940=CARTESIAN_POINT('Ctrl Pts',(7.82594753272231,2.84862442790699,-2.29809333657086));
#5941=CARTESIAN_POINT('Ctrl Pts',(7.88680439671883,2.84862442585767,-2.48054602253814));
#5942=CARTESIAN_POINT('Ctrl Pts',(7.9568078251961,2.84862442585767,-2.67630772013523));
#5943=CARTESIAN_POINT('Ctrl Pts',(7.96262190913101,2.84862442585767,-2.69246710814726));
#5944=CARTESIAN_POINT('Ctrl Pts',(7.96846622824932,2.84862442585767,-2.70861444779752));
#5945=CARTESIAN_POINT('',(7.36626248314343,2.84862442585767,-1.50713517738359));
#5946=CARTESIAN_POINT('',(13.3346225254169,2.84862442585767,-1.50713517738359));
#5947=CARTESIAN_POINT('',(6.90165952967598,2.84683860184717,-2.71030114856527));
#5948=CARTESIAN_POINT('Ctrl Pts',(6.90179278226525,2.84862442585767,-2.70862417070381));
#5949=CARTESIAN_POINT('Ctrl Pts',(6.90879787011014,2.84862442585767,-2.69252827167807));
#5950=CARTESIAN_POINT('Ctrl Pts',(6.91578301488098,2.84862442585767,-2.67642218671447));
#5951=CARTESIAN_POINT('Ctrl Pts',(7.00035932483387,2.84862442585767,-2.48070513252597));
#5952=CARTESIAN_POINT('Ctrl Pts',(7.07623460400956,2.84862442731428,-2.29789823886797));
#5953=CARTESIAN_POINT('Ctrl Pts',(7.2254662314708,2.84862442731428,-1.91583265203173));
#5954=CARTESIAN_POINT('Ctrl Pts',(7.29997769023056,2.84862442585767,-1.71136142955089));
#5955=CARTESIAN_POINT('Ctrl Pts',(7.36626248314343,2.84862442585767,-1.50713517738359));
#5956=CARTESIAN_POINT('',(6.71833248376568,2.84683991849914,-2.71030194736627));
#5957=CARTESIAN_POINT('',(11.0238490761438,2.84862442585767,-2.71179421793157));
#5958=CARTESIAN_POINT('',(6.36280938168963,2.84862442585767,-1.50713517738358));
#5959=CARTESIAN_POINT('Ctrl Pts',(6.36280938168963,2.84862442585767,-1.50713517738361));
#5960=CARTESIAN_POINT('Ctrl Pts',(6.40685906180869,2.84862442585767,-1.71160276636274));
#5961=CARTESIAN_POINT('Ctrl Pts',(6.46087159177102,2.84862442789636,-1.91525079649567));
#5962=CARTESIAN_POINT('Ctrl Pts',(6.57594597610578,2.84862442789636,-2.29809607725535));
#5963=CARTESIAN_POINT('Ctrl Pts',(6.63680259900565,2.84862442585767,-2.48055085796017));
#5964=CARTESIAN_POINT('Ctrl Pts',(6.70680637511918,2.84862442585767,-2.67631634173415));
#5965=CARTESIAN_POINT('Ctrl Pts',(6.71262089204982,2.84862442585767,-2.69247715675436));
#5966=CARTESIAN_POINT('Ctrl Pts',(6.7184656491878,2.84862442585767,-2.70862592165798));
#5967=CARTESIAN_POINT('',(6.11626248314343,2.84862442585767,-1.50713517738359));
#5968=CARTESIAN_POINT('',(13.3346225254169,2.84862442585767,-1.50713517738359));
#5969=CARTESIAN_POINT('',(5.65165950412196,2.84684801050811,-2.71030683049491));
#5970=CARTESIAN_POINT('Ctrl Pts',(5.6517921444683,2.84862442585767,-2.70863662146848));
#5971=CARTESIAN_POINT('Ctrl Pts',(5.65879781670129,2.84862442585767,-2.69253919463776));
#5972=CARTESIAN_POINT('Ctrl Pts',(5.66578354227913,2.84862442585766,-2.67643158029353));
#5973=CARTESIAN_POINT('Ctrl Pts',(5.75036060425611,2.84862442585766,-2.48071041137392));
#5974=CARTESIAN_POINT('Ctrl Pts',(5.82623584147821,2.84862442730604,-2.29790131019802));
#5975=CARTESIAN_POINT('Ctrl Pts',(5.97546697324722,2.84862442730604,-1.91583259505172));
#5976=CARTESIAN_POINT('Ctrl Pts',(6.04997762653236,2.84862442585767,-1.71136162580774));
#5977=CARTESIAN_POINT('Ctrl Pts',(6.11626248314343,2.84862442585767,-1.50713517738359));
#5978=CARTESIAN_POINT('',(5.46833245638334,2.84684948013669,-2.71030771276995));
#5979=CARTESIAN_POINT('',(11.0238490761438,2.84862442585767,-2.71179421793157));
#5980=CARTESIAN_POINT('',(5.11280938168963,2.84862442585767,-1.50713517738358));
#5981=CARTESIAN_POINT('Ctrl Pts',(5.11280938168963,2.84862442585767,-1.50713517738362));
#5982=CARTESIAN_POINT('Ctrl Pts',(5.15685909298675,2.84862442585767,-1.7116029110835));
#5983=CARTESIAN_POINT('Ctrl Pts',(5.2108708287094,2.84862442788461,-1.91525079354619));
#5984=CARTESIAN_POINT('Ctrl Pts',(5.3259442495258,2.84862442788461,-2.2980990953389));
#5985=CARTESIAN_POINT('Ctrl Pts',(5.38680060232149,2.84862442585766,-2.48055617216051));
#5986=CARTESIAN_POINT('Ctrl Pts',(5.45680476378349,2.84862442585766,-2.67632582520572));
#5987=CARTESIAN_POINT('Ctrl Pts',(5.46261975920138,2.84862442585767,-2.69248821564317));
#5988=CARTESIAN_POINT('Ctrl Pts',(5.46846500040038,2.84862442585767,-2.70863855402171));
#5989=CARTESIAN_POINT('',(4.86626248314343,2.84862442585767,-1.50713517738359));
#5990=CARTESIAN_POINT('',(13.3346225254169,2.84862442585767,-1.50713517738359));
#5991=CARTESIAN_POINT('',(4.40165946490359,2.84685854333648,-2.71031312384306));
#5992=CARTESIAN_POINT('Ctrl Pts',(4.40179142571374,2.84862442585767,-2.7086504020624));
#5993=CARTESIAN_POINT('Ctrl Pts',(4.40879774794817,2.84862442585767,-2.69255127864938));
#5994=CARTESIAN_POINT('Ctrl Pts',(4.41578411952675,2.84862442585767,-2.67644196595571));
#5995=CARTESIAN_POINT('Ctrl Pts',(4.50036202302706,2.84862442585767,-2.48071624117288));
#5996=CARTESIAN_POINT('Ctrl Pts',(4.5762372128446,2.84862442729694,-2.29790470877537));
#5997=CARTESIAN_POINT('Ctrl Pts',(4.72546780048414,2.84862442729694,-1.91583252461549));
#5998=CARTESIAN_POINT('Ctrl Pts',(4.79997755364427,2.84862442585767,-1.71136185037904));
#5999=CARTESIAN_POINT('Ctrl Pts',(4.86626248314343,2.84862442585767,-1.50713517738359));
#6000=CARTESIAN_POINT('',(4.21833241485052,2.84686019513654,-2.71031410479295));
#6001=CARTESIAN_POINT('',(11.0238490761438,2.84862442585767,-2.71179421793157));
#6002=CARTESIAN_POINT('',(3.86280938168963,2.84862442585767,-1.50713517738358));
#6003=CARTESIAN_POINT('Ctrl Pts',(3.86280938168963,2.84862442585767,-1.50713517738361));
#6004=CARTESIAN_POINT('Ctrl Pts',(3.90685912895696,2.84862442585767,-1.71160307804822));
#6005=CARTESIAN_POINT('Ctrl Pts',(3.9608699742735,2.84862442787157,-1.91525078515163));
#6006=CARTESIAN_POINT('Ctrl Pts',(4.07594232175518,2.84862442787157,-2.29810243978791));
#6007=CARTESIAN_POINT('Ctrl Pts',(4.13679836986563,2.84862442585768,-2.48056204862024));
#6008=CARTESIAN_POINT('Ctrl Pts',(4.20680296129537,2.84862442585768,-2.67633632166697));
#6009=CARTESIAN_POINT('Ctrl Pts',(4.21261848888836,2.84862442585767,-2.69250046252893));
#6010=CARTESIAN_POINT('Ctrl Pts',(4.21846426848655,2.84862442585767,-2.70865254916597));
#6011=CARTESIAN_POINT('',(3.61626248314343,2.84862442585767,-1.50713517738359));
#6012=CARTESIAN_POINT('',(13.3346225254169,2.84862442585767,-1.50713517738359));
#6013=CARTESIAN_POINT('',(3.15165940830577,2.8468704213803,-2.71032014357828));
#6014=CARTESIAN_POINT('Ctrl Pts',(3.15179060954266,2.84862442585767,-2.70866576166606));
#6015=CARTESIAN_POINT('Ctrl Pts',(3.15879766001169,2.84862442585767,-2.69256474069428));
#6016=CARTESIAN_POINT('Ctrl Pts',(3.1657847553136,2.84862442585768,-2.6764535284648));
#6017=CARTESIAN_POINT('Ctrl Pts',(3.25036360752406,2.84862442585768,-2.48072272386991));
#6018=CARTESIAN_POINT('Ctrl Pts',(3.32623874336682,2.84862442728679,-2.29790849584301));
#6019=CARTESIAN_POINT('Ctrl Pts',(3.4754687298166,2.84862442728679,-1.91583243746613));
#6020=CARTESIAN_POINT('Ctrl Pts',(3.54997746960448,2.84862442585767,-1.71136210930917));
#6021=CARTESIAN_POINT('Ctrl Pts',(3.61626248314343,2.84862442585767,-1.50713517738359));
#6022=CARTESIAN_POINT('',(3.02384907614375,2.84862442585767,-2.71179421793157));
#6023=CARTESIAN_POINT('',(11.0238490761438,2.84862442585767,-2.71179421793157));
#6024=CARTESIAN_POINT('',(3.02384907614375,2.84862442585767,2.11350930841789));
#6025=CARTESIAN_POINT('',(3.02384907614375,2.84862442585767,1.40404227860195));
#6026=CARTESIAN_POINT('',(3.27141298814991,2.84845804217612,2.71158690494159));
#6027=CARTESIAN_POINT('Ctrl Pts',(3.27100497985698,2.84862442585767,2.71079938718163));
#6028=CARTESIAN_POINT('Ctrl Pts',(3.228076353399,2.84862442585767,2.61225572759565));
#6029=CARTESIAN_POINT('Ctrl Pts',(3.18578823704266,2.84862442598707,2.51303020389064));
#6030=CARTESIAN_POINT('Ctrl Pts',(3.10334913028736,2.84862442598707,2.31421002248986));
#6031=CARTESIAN_POINT('Ctrl Pts',(3.06291723376633,2.84862442585767,2.21392684695503));
#6032=CARTESIAN_POINT('Ctrl Pts',(3.02384907614376,2.84862442585767,2.11350930841789));
#6033=CARTESIAN_POINT('',(3.45436575618682,2.84686429810077,2.7103165345807));
#6034=CARTESIAN_POINT('',(11.0238490761438,2.84862442585767,2.71179421793157));
#6035=CARTESIAN_POINT('',(3.80988877059788,2.84862442585767,1.5071351773836));
#6036=CARTESIAN_POINT('Ctrl Pts',(3.80988877059788,2.84862442585767,1.5071351773836));
#6037=CARTESIAN_POINT('Ctrl Pts',(3.7658293274531,2.84862442585767,1.71164808388438));
#6038=CARTESIAN_POINT('Ctrl Pts',(3.7118046719511,2.84862442781797,1.9153406753387));
#6039=CARTESIAN_POINT('Ctrl Pts',(3.59671531847852,2.84862442781797,2.29823125790659));
#6040=CARTESIAN_POINT('Ctrl Pts',(3.53585880786088,2.84862442585766,2.48068659685609));
#6041=CARTESIAN_POINT('Ctrl Pts',(3.46586775948282,2.84862442585766,2.67641846844891));
#6042=CARTESIAN_POINT('Ctrl Pts',(3.46006601698536,2.84862442585767,2.69254416467973));
#6043=CARTESIAN_POINT('Ctrl Pts',(3.45423416535493,2.84862442585767,2.7086578664456));
#6044=CARTESIAN_POINT('',(4.05643566914408,2.84862442585766,1.50713517738361));
#6045=CARTESIAN_POINT('',(13.3346225254169,2.84862442585767,1.50713517738359));
#6046=CARTESIAN_POINT('',(4.52103867175434,2.84685468053191,2.71031082368787));
#6047=CARTESIAN_POINT('Ctrl Pts',(4.52090646241579,2.84862442585767,2.70864536656847));
#6048=CARTESIAN_POINT('Ctrl Pts',(4.51389718302579,2.84862442585767,2.69253952221217));
#6049=CARTESIAN_POINT('Ctrl Pts',(4.50690787077022,2.84862442585768,2.67642347934393));
#6050=CARTESIAN_POINT('Ctrl Pts',(4.42232697249459,2.84862442585768,2.48069113060106));
#6051=CARTESIAN_POINT('Ctrl Pts',(4.34645166843461,2.84862442738707,2.29787949083546));
#6052=CARTESIAN_POINT('Ctrl Pts',(4.19722448429369,2.84862442738707,1.91581561039782));
#6053=CARTESIAN_POINT('Ctrl Pts',(4.12271784469148,2.84862442585767,1.7113533653371));
#6054=CARTESIAN_POINT('Ctrl Pts',(4.05643566914409,2.84862442585767,1.50713517738361));
#6055=CARTESIAN_POINT('',(4.70436570878572,2.84685312375625,2.71030989419369));
#6056=CARTESIAN_POINT('',(11.0238490761438,2.84862442585767,2.71179421793157));
#6057=CARTESIAN_POINT('',(5.05988877059788,2.84862442585767,1.5071351773836));
#6058=CARTESIAN_POINT('Ctrl Pts',(5.05988877059787,2.84862442585767,1.50713517738362));
#6059=CARTESIAN_POINT('Ctrl Pts',(5.01582936546295,2.84862442585767,1.71164790745213));
#6060=CARTESIAN_POINT('Ctrl Pts',(4.96180378091768,2.84862442783138,1.91534068528627));
#6061=CARTESIAN_POINT('Ctrl Pts',(4.84671331029461,2.84862442783138,2.29822778278234));
#6062=CARTESIAN_POINT('Ctrl Pts',(4.78585648120188,2.84862442585767,2.48068049652974));
#6063=CARTESIAN_POINT('Ctrl Pts',(4.71586588068668,2.84862442585767,2.6764075700122));
#6064=CARTESIAN_POINT('Ctrl Pts',(4.71006469178374,2.84862442585767,2.69253144678897));
#6065=CARTESIAN_POINT('Ctrl Pts',(4.70423340021296,2.84862442585767,2.70864333135427));
#6066=CARTESIAN_POINT('',(5.30643566914408,2.84862442585766,1.50713517738361));
#6067=CARTESIAN_POINT('',(13.3346225254169,2.84862442585767,1.50713517738359));
#6068=CARTESIAN_POINT('',(5.77103863773745,2.8468445674932,2.71030475813399));
#6069=CARTESIAN_POINT('Ctrl Pts',(5.77090577394363,2.84862442585767,2.70863208133986));
#6070=CARTESIAN_POINT('Ctrl Pts',(5.7638971201788,2.84862442585767,2.69252787095137));
#6071=CARTESIAN_POINT('Ctrl Pts',(5.75690842970124,2.84862442585768,2.67641346374591));
#6072=CARTESIAN_POINT('Ctrl Pts',(5.67232833961162,2.84862442585768,2.48068550687512));
#6073=CARTESIAN_POINT('Ctrl Pts',(5.59645299018697,2.84862442739611,2.29787621515313));
#6074=CARTESIAN_POINT('Ctrl Pts',(5.44722527981436,2.84862442739611,1.91581567641076));
#6075=CARTESIAN_POINT('Ctrl Pts',(5.3727177753678,2.84862442585767,1.71135315174791));
#6076=CARTESIAN_POINT('Ctrl Pts',(5.30643566914408,2.84862442585767,1.5071351773836));
#6077=CARTESIAN_POINT('',(5.95436567678183,2.84684317743142,2.71030391927272));
#6078=CARTESIAN_POINT('',(11.0238490761438,2.84862442585767,2.71179421793157));
#6079=CARTESIAN_POINT('',(6.30988877059788,2.84862442585767,1.5071351773836));
#6080=CARTESIAN_POINT('Ctrl Pts',(6.30988877059789,2.84862442585767,1.5071351773836));
#6081=CARTESIAN_POINT('Ctrl Pts',(6.2658293983268,2.84862442585767,1.71164775490643));
#6082=CARTESIAN_POINT('Ctrl Pts',(6.21180298721187,2.84862442784341,1.91534068936543));
#6083=CARTESIAN_POINT('Ctrl Pts',(6.09671151624063,2.84862442784341,2.29822465435504));
#6084=CARTESIAN_POINT('Ctrl Pts',(6.03585440555947,2.84862442585767,2.48067499299047));
#6085=CARTESIAN_POINT('Ctrl Pts',(5.96586420541966,2.84862442585767,2.67639774691987));
#6086=CARTESIAN_POINT('Ctrl Pts',(5.96006351303068,2.84862442585767,2.69251999018277));
#6087=CARTESIAN_POINT('Ctrl Pts',(5.95423272375062,2.84862442585767,2.70863024324505));
#6088=CARTESIAN_POINT('',(6.55643566914408,2.84862442585766,1.50713517738361));
#6089=CARTESIAN_POINT('',(13.3346225254169,2.84862442585767,1.50713517738359));
#6090=CARTESIAN_POINT('',(7.02103861629541,2.84683551225861,2.71029926942148));
#6091=CARTESIAN_POINT('Ctrl Pts',(7.02090516150519,2.84862442585767,2.70862005097967));
#6092=CARTESIAN_POINT('Ctrl Pts',(7.01389707152942,2.84862442585767,2.69251731541987));
#6093=CARTESIAN_POINT('Ctrl Pts',(7.0069089413909,2.84862442585767,2.67640438456248));
#6094=CARTESIAN_POINT('Ctrl Pts',(6.92232957528187,2.84862442585767,2.48068040331129));
#6095=CARTESIAN_POINT('Ctrl Pts',(6.84645418560907,2.84862442740432,2.29787324819636));
#6096=CARTESIAN_POINT('Ctrl Pts',(6.6972259948484,2.84862442740432,1.91581572986742));
#6097=CARTESIAN_POINT('Ctrl Pts',(6.62271771463721,2.84862442585767,1.71135296463439));
#6098=CARTESIAN_POINT('Ctrl Pts',(6.55643566914408,2.84862442585767,1.5071351773836));
#6099=CARTESIAN_POINT('',(7.20436565693214,2.84683426291388,2.71029850763795));
#6100=CARTESIAN_POINT('',(11.0238490761438,2.84862442585767,2.71179421793157));
#6101=CARTESIAN_POINT('',(7.55988877059788,2.84862442585767,1.5071351773836));
#6102=CARTESIAN_POINT('Ctrl Pts',(7.55988877059788,2.84862442585767,1.5071351773836));
#6103=CARTESIAN_POINT('Ctrl Pts',(7.51582942694069,2.84862442585767,1.71164762208787));
#6104=CARTESIAN_POINT('Ctrl Pts',(7.46180227524923,2.84862442785429,1.91534068886327));
#6105=CARTESIAN_POINT('Ctrl Pts',(7.34670990240678,2.84862442785429,2.29822181949426));
#6106=CARTESIAN_POINT('Ctrl Pts',(7.28585254096374,2.84862442585767,2.48066999572136));
#6107=CARTESIAN_POINT('Ctrl Pts',(7.2158627012126,2.84862442585767,2.67638883532302));
#6108=CARTESIAN_POINT('Ctrl Pts',(7.21006245715211,2.84862442585767,2.69250960216246));
#6109=CARTESIAN_POINT('Ctrl Pts',(7.20423212139549,2.84862442585767,2.70861838061489));
#6110=CARTESIAN_POINT('',(7.80643566914408,2.84862442585766,1.50713517738361));
#6111=CARTESIAN_POINT('',(13.3346225254169,2.84862442585767,1.50713517738359));
#6112=CARTESIAN_POINT('',(8.27103860483754,2.84682735344229,2.71029427328957));
#6113=CARTESIAN_POINT('Ctrl Pts',(8.27090461316402,2.84862442585767,2.70860909277273));
#6114=CARTESIAN_POINT('Ctrl Pts',(8.26389703435909,2.84862442585767,2.69250769644918));
#6115=CARTESIAN_POINT('Ctrl Pts',(8.25690941227972,2.84862442585767,2.67639610620256));
#6116=CARTESIAN_POINT('Ctrl Pts',(8.17233069882605,2.84862442585767,2.48067574504101));
#6117=CARTESIAN_POINT('Ctrl Pts',(8.0964552732107,2.84862442741179,2.29787054506796));
#6118=CARTESIAN_POINT('Ctrl Pts',(7.94722664153419,2.84862442741179,1.91581577309339));
#6119=CARTESIAN_POINT('Ctrl Pts',(7.87271766108794,2.84862442585767,1.71135279964682));
#6120=CARTESIAN_POINT('Ctrl Pts',(7.80643566914409,2.84862442585767,1.50713517738362));
#6121=CARTESIAN_POINT('',(8.45436564674126,2.84682622399784,2.71029357769283));
#6122=CARTESIAN_POINT('',(11.0238490761438,2.84862442585767,2.71179421793157));
#6123=CARTESIAN_POINT('',(8.80988877059788,2.84862442585767,1.50713517738359));
#6124=CARTESIAN_POINT('Ctrl Pts',(8.80988877059788,2.84862442585767,1.50713517738359));
#6125=CARTESIAN_POINT('Ctrl Pts',(8.76582945201024,2.84862442585767,1.7116475057213));
#6126=CARTESIAN_POINT('Ctrl Pts',(8.71180163264592,2.84862442786418,1.91534068476964));
#6127=CARTESIAN_POINT('Ctrl Pts',(8.59670844181264,2.84862442786418,2.29821923576154));
#6128=CARTESIAN_POINT('Ctrl Pts',(8.53585085563285,2.84862442585767,2.48066543233191));
#6129=CARTESIAN_POINT('Ctrl Pts',(8.46586134225275,2.84862442585767,2.67638070425965));
#6130=CARTESIAN_POINT('Ctrl Pts',(8.46006150542514,2.84862442585767,2.69250012875935));
#6131=CARTESIAN_POINT('Ctrl Pts',(8.45423158160217,2.84862442585767,2.70860756651644));
#6132=CARTESIAN_POINT('',(9.05643566914408,2.84862442585766,1.50713517738361));
#6133=CARTESIAN_POINT('',(13.3346225254169,2.84862442585767,1.50713517738359));
#6134=CARTESIAN_POINT('',(9.52103860134977,2.8468199611698,2.71028970168337));
#6135=CARTESIAN_POINT('Ctrl Pts',(9.52090411935796,2.84862442585767,2.70859905909218));
#6136=CARTESIAN_POINT('Ctrl Pts',(9.51389700653417,2.84862442585767,2.69249888540408));
#6137=CARTESIAN_POINT('Ctrl Pts',(9.50690984761346,2.84862442585768,2.67638851904301));
#6138=CARTESIAN_POINT('Ctrl Pts',(9.42233172583661,2.84862442585768,2.48067147148852));
#6139=CARTESIAN_POINT('Ctrl Pts',(9.3464562679359,2.84862442741865,2.29786806948615));
#6140=CARTESIAN_POINT('Ctrl Pts',(9.19722722963917,2.84862442741865,1.9158158079193));
#6141=CARTESIAN_POINT('Ctrl Pts',(9.12271761359435,2.84862442585767,1.71135265331708));
#6142=CARTESIAN_POINT('Ctrl Pts',(9.05643566914409,2.84862442585767,1.50713517738362));
#6143=CARTESIAN_POINT('',(9.70436564426604,2.84681893475664,2.71028906341284));
#6144=CARTESIAN_POINT('',(11.0238490761438,2.84862442585767,2.71179421793157));
#6145=CARTESIAN_POINT('',(10.0598887705979,2.84862442585767,1.50713517738359));
#6146=CARTESIAN_POINT('Ctrl Pts',(10.0598887705979,2.84862442585767,1.50713517738359));
#6147=CARTESIAN_POINT('Ctrl Pts',(10.0158294740978,2.84862442585767,1.71164740319615));
#6148=CARTESIAN_POINT('Ctrl Pts',(9.96180104943227,2.84862442787322,1.91534067785543));
#6149=CARTESIAN_POINT('Ctrl Pts',(9.84670711270893,2.84862442787322,2.29821686881042));
#6150=CARTESIAN_POINT('Ctrl Pts',(9.78584932396424,2.84862442585767,2.48066124415883));
#6151=CARTESIAN_POINT('Ctrl Pts',(9.71586010775059,2.84862442585767,2.67637324766241));
#6152=CARTESIAN_POINT('Ctrl Pts',(9.71006064278651,2.84862442585767,2.69249144531452));
#6153=CARTESIAN_POINT('Ctrl Pts',(9.70423109510515,2.84862442585767,2.70859765771964));
#6154=CARTESIAN_POINT('',(10.3064356691441,2.84862442585766,1.50713517738361));
#6155=CARTESIAN_POINT('',(13.3346225254169,2.84862442585767,1.50713517738359));
#6156=CARTESIAN_POINT('',(10.7710386042496,2.84681322972354,2.71028549897447));
#6157=CARTESIAN_POINT('Ctrl Pts',(10.7709036723368,2.84862442585767,2.70858982922371));
#6158=CARTESIAN_POINT('Ctrl Pts',(10.7638969863635,2.84862442585767,2.69249077707409));
#6159=CARTESIAN_POINT('Ctrl Pts',(10.7569102517173,2.84862442585767,2.67638153338721));
#6160=CARTESIAN_POINT('Ctrl Pts',(10.6723326690498,2.84862442585767,2.48066753305333));
#6161=CARTESIAN_POINT('Ctrl Pts',(10.5964571819956,2.84862442742496,2.29786579177956));
#6162=CARTESIAN_POINT('Ctrl Pts',(10.4472277671172,2.84862442742496,1.91581583580293));
#6163=CARTESIAN_POINT('Ctrl Pts',(10.3727175712488,2.84862442585767,1.71135252284851));
#6164=CARTESIAN_POINT('Ctrl Pts',(10.3064356691441,2.84862442585767,1.5071351773836));
#6165=CARTESIAN_POINT('',(10.9543681768003,2.84860418144656,2.71177492056083));
#6166=CARTESIAN_POINT('',(11.0238490761438,2.84862442585767,2.71179421793157));
#6167=CARTESIAN_POINT('',(11.0238490761438,2.84862442585767,2.5145657703754));
#6168=CARTESIAN_POINT('Ctrl Pts',(11.0238490761438,2.84862442585767,2.51456577037539));
#6169=CARTESIAN_POINT('Ctrl Pts',(11.0125388019847,2.84862442585767,2.54755700411209));
#6170=CARTESIAN_POINT('Ctrl Pts',(11.0010794330984,2.84862442585774,2.58050639119045));
#6171=CARTESIAN_POINT('Ctrl Pts',(10.9781080325486,2.84862442585774,2.6456791051022));
#6172=CARTESIAN_POINT('Ctrl Pts',(10.9665953160741,2.84862442585767,2.67792052124666));
#6173=CARTESIAN_POINT('Ctrl Pts',(10.9547630945647,2.84862442585767,2.71065726237697));
#6174=CARTESIAN_POINT('Ctrl Pts',(10.9545649113151,2.84862442585767,2.71120547217373));
#6175=CARTESIAN_POINT('Ctrl Pts',(10.9543666920789,2.84862442585767,2.71175366890678));
#6176=CARTESIAN_POINT('',(11.0238490761438,2.84862442585767,-6.75363122348402));
#6177=CARTESIAN_POINT('Origin',(13.3346225254169,0.,0.));
#6178=CARTESIAN_POINT('',(3.02409152551386,-0.0272219868854266,3.22221592290483));
#6179=CARTESIAN_POINT('Ctrl Pts',(3.23780938168962,-2.84862442585767,1.50713517738359));
#6180=CARTESIAN_POINT('Ctrl Pts',(3.22442453716735,-2.74722502408512,1.69878939459725));
#6181=CARTESIAN_POINT('Ctrl Pts',(3.21148030385348,-2.62674430926649,1.87972173710279));
#6182=CARTESIAN_POINT('Ctrl Pts',(3.18515854827395,-2.35116852031272,2.21476896718337));
#6183=CARTESIAN_POINT('Ctrl Pts',(3.17183872397072,-2.19678014965427,2.36798232659674));
#6184=CARTESIAN_POINT('Ctrl Pts',(3.1491421401168,-1.91598526745743,2.59537315704631));
#6185=CARTESIAN_POINT('Ctrl Pts',(3.13997414564689,-1.79781120104803,2.6785880739654));
#6186=CARTESIAN_POINT('Ctrl Pts',(3.11246007094934,-1.42767513520865,2.90366763005427));
#6187=CARTESIAN_POINT('Ctrl Pts',(3.09467202235144,-1.16180919607831,3.01989665639061));
#6188=CARTESIAN_POINT('Ctrl Pts',(3.05986689150469,-0.605250308275812,3.17864929438211));
#6189=CARTESIAN_POINT('Ctrl Pts',(3.04244620156952,-0.317070870595313,3.22018452284352));
#6190=CARTESIAN_POINT('Ctrl Pts',(3.0243364807485,-0.0272455238111505,3.22263482944194));
#6191=CARTESIAN_POINT('Origin',(3.02384907614375,0.,0.));
#6192=CARTESIAN_POINT('Origin',(13.3346225254169,0.,0.));
#6193=CARTESIAN_POINT('Ctrl Pts',(3.61626248314344,2.84862442585767,-1.50713517738358));
#6194=CARTESIAN_POINT('Ctrl Pts',(3.59307108387217,2.67293362807053,-1.83920698188073));
#6195=CARTESIAN_POINT('Ctrl Pts',(3.56888016255196,2.44052702935851,-2.13802203875356));
#6196=CARTESIAN_POINT('Ctrl Pts',(3.52292662769557,1.88507649015484,-2.64043283240736));
#6197=CARTESIAN_POINT('Ctrl Pts',(3.50145575366532,1.56693992247333,-2.84078534752095));
#6198=CARTESIAN_POINT('Ctrl Pts',(3.45301242989295,0.83394564202971,-3.14104684531098));
#6199=CARTESIAN_POINT('Ctrl Pts',(3.42556936284725,0.419015787858895,-3.22274339729798));
#6200=CARTESIAN_POINT('Ctrl Pts',(3.37393448273109,-0.418922408506109,-3.22275660206917));
#6201=CARTESIAN_POINT('Ctrl Pts',(3.35014729256515,-0.833858370849191,-3.14106853204561));
#6202=CARTESIAN_POINT('Ctrl Pts',(3.30059617351017,-1.56685554891026,-2.84083243276982));
#6203=CARTESIAN_POINT('Ctrl Pts',(3.27632232182658,-1.8850119004154,-2.6404833146547));
#6204=CARTESIAN_POINT('Ctrl Pts',(3.22990333374809,-2.44049642846581,-2.13805771006364));
#6205=CARTESIAN_POINT('Ctrl Pts',(3.20808192590441,-2.67292032489589,-1.83923212610718));
#6206=CARTESIAN_POINT('Ctrl Pts',(3.18488877059789,-2.84862442585765,-1.50713517738362));
#6207=CARTESIAN_POINT('Ctrl Pts',(3.86280938168963,2.84862442585767,-1.50713517738358));
#6208=CARTESIAN_POINT('Ctrl Pts',(3.83961637099924,2.67292142046256,-1.83923005538518));
#6209=CARTESIAN_POINT('Ctrl Pts',(3.81779859998544,2.4404992595268,-2.13805411438247));
#6210=CARTESIAN_POINT('Ctrl Pts',(3.77138581521096,1.88501876089811,-2.6404781375374));
#6211=CARTESIAN_POINT('Ctrl Pts',(3.74711428478802,1.56686481641917,-2.84082703445761));
#6212=CARTESIAN_POINT('Ctrl Pts',(3.69756239352038,0.833866711494175,-3.14106691461616));
#6213=CARTESIAN_POINT('Ctrl Pts',(3.67377245274625,0.418926363378426,-3.22275665847088));
#6214=CARTESIAN_POINT('Ctrl Pts',(3.62213600150572,-0.419020559361353,-3.2227433408852));
#6215=CARTESIAN_POINT('Ctrl Pts',(3.59469416940512,-0.833954782426799,-3.14104502062188));
#6216=CARTESIAN_POINT('Ctrl Pts',(3.5462514514891,-1.56694997159161,-2.84077952129024));
#6217=CARTESIAN_POINT('Ctrl Pts',(3.5247792040526,-1.88508393374335,-2.64042719604862));
#6218=CARTESIAN_POINT('Ctrl Pts',(3.47882096430004,-2.44052993660295,-2.13801830515755));
#6219=CARTESIAN_POINT('Ctrl Pts',(3.45462692413533,-2.67293472109094,-1.83920491597139));
#6220=CARTESIAN_POINT('Ctrl Pts',(3.43143566914409,-2.84862442585767,-1.5071351773836));
#6221=CARTESIAN_POINT('Origin',(13.3346225254169,0.,0.));
#6222=CARTESIAN_POINT('Ctrl Pts',(4.48780938168963,-2.84862442585767,1.50713517738358));
#6223=CARTESIAN_POINT('Ctrl Pts',(4.46461645011834,-2.6729220198441,1.83922892249882));
#6224=CARTESIAN_POINT('Ctrl Pts',(4.44280064601111,-2.44050080835351,2.13805214696681));
#6225=CARTESIAN_POINT('Ctrl Pts',(4.39639124959945,-1.88502246104519,2.64047535351999));
#6226=CARTESIAN_POINT('Ctrl Pts',(4.37212100669442,-1.56686976109429,2.84082416041238));
#6227=CARTESIAN_POINT('Ctrl Pts',(4.32256878074722,-0.833871112828827,3.14106606462272));
#6228=CARTESIAN_POINT('Ctrl Pts',(4.29877739278441,-0.418928424370983,3.22275669480111));
#6229=CARTESIAN_POINT('Ctrl Pts',(4.24714010625329,0.419023153943,3.22274330454761));
#6230=CARTESIAN_POINT('Ctrl Pts',(4.21969891604846,0.833959705309191,3.14104403448372));
#6231=CARTESIAN_POINT('Ctrl Pts',(4.17125644341379,1.56695540238117,2.84077637878877));
#6232=CARTESIAN_POINT('Ctrl Pts',(4.14978340883144,1.88508799604372,2.64042412833943));
#6233=CARTESIAN_POINT('Ctrl Pts',(4.10382257494227,2.44053154431161,2.13801624010711));
#6234=CARTESIAN_POINT('Ctrl Pts',(4.07962684434337,2.67293532556987,1.83920377345047));
#6235=CARTESIAN_POINT('Ctrl Pts',(4.05643566914409,2.84862442585766,1.5071351773836));
#6236=CARTESIAN_POINT('Ctrl Pts',(4.24126248314343,-2.84862442585767,1.50713517738358));
#6237=CARTESIAN_POINT('Ctrl Pts',(4.21807117017573,-2.6729342818794,1.83920574612168));
#6238=CARTESIAN_POINT('Ctrl Pts',(4.19387838424026,-2.44052876832755,2.13801980560761));
#6239=CARTESIAN_POINT('Ctrl Pts',(4.14792204906491,-1.88508095777294,2.64042944713896));
#6240=CARTESIAN_POINT('Ctrl Pts',(4.12645036612162,-1.56694596905136,2.84078184008319));
#6241=CARTESIAN_POINT('Ctrl Pts',(4.07800742879564,-0.833951160700149,3.14104574166853));
#6242=CARTESIAN_POINT('Ctrl Pts',(4.05056510798455,-0.419018684053894,3.2227433592853));
#6243=CARTESIAN_POINT('Ctrl Pts',(3.99892928355449,0.418924751693643,3.22275664007429));
#6244=CARTESIAN_POINT('Ctrl Pts',(3.97514043617366,0.833863348516512,3.14106756893928));
#6245=CARTESIAN_POINT('Ctrl Pts',(3.92558883146838,1.56686108050826,2.84082920882958));
#6246=CARTESIAN_POINT('Ctrl Pts',(3.90131635909468,1.88501598412944,2.64048023071256));
#6247=CARTESIAN_POINT('Ctrl Pts',(3.85490107229755,2.44049810801134,2.13805557711095));
#6248=CARTESIAN_POINT('Ctrl Pts',(3.8330818401007,2.67292097491792,1.83923089750562));
#6249=CARTESIAN_POINT('Ctrl Pts',(3.80988877059788,2.84862442585767,1.5071351773836));
#6250=CARTESIAN_POINT('Origin',(13.3346225254169,0.,0.));
#6251=CARTESIAN_POINT('Ctrl Pts',(4.86626248314343,2.84862442585767,-1.50713517738359));
#6252=CARTESIAN_POINT('Ctrl Pts',(4.84307125255646,2.6729349059701,-1.83920456653272));
#6253=CARTESIAN_POINT('Ctrl Pts',(4.81887670737099,2.44053042821952,-2.13801767372441));
#6254=CARTESIAN_POINT('Ctrl Pts',(4.77291769607632,1.88508518038666,-2.64042625393169));
#6255=CARTESIAN_POINT('Ctrl Pts',(4.75144521687828,1.56695164272654,-2.84077855370853));
#6256=CARTESIAN_POINT('Ctrl Pts',(4.70300257961491,0.833956318311138,-3.14104470921497));
#6257=CARTESIAN_POINT('Ctrl Pts',(4.67556094159899,0.419021397612177,-3.22274332225382));
#6258=CARTESIAN_POINT('Ctrl Pts',(4.62392423900021,-0.418926923466486,-3.22275667709832));
#6259=CARTESIAN_POINT('Ctrl Pts',(4.60013386197003,-0.833867976385865,-3.14106667450484));
#6260=CARTESIAN_POINT('Ctrl Pts',(4.55058186393659,-1.56686625632318,-2.84082619705477));
#6261=CARTESIAN_POINT('Ctrl Pts',(4.52631071569599,-1.88501983574479,-2.64047732835315));
#6262=CARTESIAN_POINT('Ctrl Pts',(4.47989894120053,-2.4404997087135,-2.13805354399739));
#6263=CARTESIAN_POINT('Ctrl Pts',(4.45808175832889,-2.67292159439562,-1.83922972663566));
#6264=CARTESIAN_POINT('Ctrl Pts',(4.43488877059788,-2.84862442585766,-1.50713517738361));
#6265=CARTESIAN_POINT('Ctrl Pts',(5.11280938168963,2.84862442585767,-1.50713517738359));
#6266=CARTESIAN_POINT('Ctrl Pts',(5.08961652572833,2.67292259264177,-1.83922783985841));
#6267=CARTESIAN_POINT('Ctrl Pts',(5.06780258054985,2.44050228855337,-2.13805026647637));
#6268=CARTESIAN_POINT('Ctrl Pts',(5.02139640928981,1.88502596245473,-2.64047272456218));
#6269=CARTESIAN_POINT('Ctrl Pts',(4.99712740512678,1.56687440390419,-2.8408214660952));
#6270=CARTESIAN_POINT('Ctrl Pts',(4.94757491926147,0.833875219125953,-3.1410652724995));
#6271=CARTESIAN_POINT('Ctrl Pts',(4.92378219113448,0.418930341135908,-3.22275673021487));
#6272=CARTESIAN_POINT('Ctrl Pts',(4.87214412512137,-0.419025593375922,-3.22274326912658));
#6273=CARTESIAN_POINT('Ctrl Pts',(4.84470352387355,-0.833964322246264,-3.1410431087264));
#6274=CARTESIAN_POINT('Ctrl Pts',(4.79626122682024,-1.56696051586174,-2.8407734241006));
#6275=CARTESIAN_POINT('Ctrl Pts',(4.77478741813673,-1.8850918479804,-2.6404212250909));
#6276=CARTESIAN_POINT('Ctrl Pts',(4.72882409875911,-2.44053308298953,-2.13801426347771));
#6277=CARTESIAN_POINT('Ctrl Pts',(4.70462676797604,-2.67293590410493,-1.83920267996586));
#6278=CARTESIAN_POINT('Ctrl Pts',(4.68143566914409,-2.84862442585766,-1.5071351773836));
#6279=CARTESIAN_POINT('Origin',(13.3346225254169,0.,0.));
#6280=CARTESIAN_POINT('Ctrl Pts',(5.73780938168963,-2.84862442585766,1.5071351773836));
#6281=CARTESIAN_POINT('Ctrl Pts',(5.71461659809079,-2.67292314083723,1.83922680371845));
#6282=CARTESIAN_POINT('Ctrl Pts',(5.69280441295107,-2.44050370523866,2.13804846644808));
#6283=CARTESIAN_POINT('Ctrl Pts',(5.64640131646479,-1.88502928166926,2.64047023752963));
#6284=CARTESIAN_POINT('Ctrl Pts',(5.62213350550393,-1.56687877146956,2.84081893550195));
#6285=CARTESIAN_POINT('Ctrl Pts',(5.57258082594982,-0.833879057355483,3.14106453292806));
#6286=CARTESIAN_POINT('Ctrl Pts',(5.54878685458684,-0.418932127052885,3.22275676474664));
#6287=CARTESIAN_POINT('Ctrl Pts',(5.49714805980877,0.419027891231812,3.22274323458767));
#6288=CARTESIAN_POINT('Ctrl Pts',(5.46970799973081,0.833968660424517,3.14104223801657));
#6289=CARTESIAN_POINT('Ctrl Pts',(5.42126581665765,1.5669653395092,2.8407706408043));
#6290=CARTESIAN_POINT('Ctrl Pts',(5.39979124701918,1.88509550674795,2.6404184726215));
#6291=CARTESIAN_POINT('Ctrl Pts',(5.35382554299669,2.44053455767071,2.13801236883365));
#6292=CARTESIAN_POINT('Ctrl Pts',(5.32962669478367,2.67293645858739,1.8392016319429));
#6293=CARTESIAN_POINT('Ctrl Pts',(5.30643566914408,2.84862442585766,1.5071351773836));
#6294=CARTESIAN_POINT('Ctrl Pts',(5.49126248314343,-2.84862442585767,1.50713517738358));
#6295=CARTESIAN_POINT('Ctrl Pts',(5.46807133131819,-2.67293550264439,1.83920343876331));
#6296=CARTESIAN_POINT('Ctrl Pts',(5.44387512300406,-2.44053201516125,2.13801563527266));
#6297=CARTESIAN_POINT('Ctrl Pts',(5.39791355030629,-1.88508917917162,2.64042323590796));
#6298=CARTESIAN_POINT('Ctrl Pts',(5.37644028777467,-1.56695697751933,2.84077546804639));
#6299=CARTESIAN_POINT('Ctrl Pts',(5.32799787444477,-0.833961148602932,3.14104374133487));
#6300=CARTESIAN_POINT('Ctrl Pts',(5.30055686222276,-0.419023945353596,3.22274328616581));
#6301=CARTESIAN_POINT('Ctrl Pts',(5.24891934126886,0.418928940489715,3.22275671317899));
#6302=CARTESIAN_POINT('Ctrl Pts',(5.22512754956627,0.83387228800949,3.14106584212302));
#6303=CARTESIAN_POINT('Ctrl Pts',(5.17557523973541,1.56687110936966,2.84082337758039));
#6304=CARTESIAN_POINT('Ctrl Pts',(5.15130536434743,1.88502347566865,2.64047459134714));
#6305=CARTESIAN_POINT('Ctrl Pts',(5.1048969289169,2.44050123680849,2.13805160284053));
#6306=CARTESIAN_POINT('Ctrl Pts',(5.08308168026985,2.6729221857465,1.83922860892797));
#6307=CARTESIAN_POINT('Ctrl Pts',(5.05988877059787,2.84862442585766,1.5071351773836));
#6308=CARTESIAN_POINT('Origin',(13.3346225254169,0.,0.));
#6309=CARTESIAN_POINT('Ctrl Pts',(6.11626248314343,2.84862442585767,-1.50713517738359));
#6310=CARTESIAN_POINT('Ctrl Pts',(6.09307140673134,2.67293607395078,-1.83920235894155));
#6311=CARTESIAN_POINT('Ctrl Pts',(6.06887362324604,2.44053353460538,-2.138013683282));
#6312=CARTESIAN_POINT('Ctrl Pts',(6.02290959541348,1.8850929728442,-2.64042037816482));
#6313=CARTESIAN_POINT('Ctrl Pts',(6.00143556263095,1.56696200340518,-2.84077256517489));
#6314=CARTESIAN_POINT('Ctrl Pts',(5.9529933060248,0.833965681264298,-3.14104283220532));
#6315=CARTESIAN_POINT('Ctrl Pts',(5.92555286823777,0.41902634209052,-3.22274325098545));
#6316=CARTESIAN_POINT('Ctrl Pts',(5.87391458317757,-0.418930817396119,-3.2227567483521));
#6317=CARTESIAN_POINT('Ctrl Pts',(5.85012148073232,-0.833876312868828,-3.1410650659791));
#6318=CARTESIAN_POINT('Ctrl Pts',(5.8005689312425,-1.56687566870931,-2.84082073292859));
#6319=CARTESIAN_POINT('Ctrl Pts',(5.77630028091622,-1.88502692192012,-2.64047200537797));
#6320=CARTESIAN_POINT('Ctrl Pts',(5.72989502526017,-2.44050269783885,-2.13804974663392));
#6321=CARTESIAN_POINT('Ctrl Pts',(5.70808160563999,-2.67292275111906,-1.83922754032172));
#6322=CARTESIAN_POINT('Ctrl Pts',(5.68488877059789,-2.84862442585766,-1.50713517738361));
#6323=CARTESIAN_POINT('Ctrl Pts',(6.36280938168962,2.84862442585767,-1.50713517738359));
#6324=CARTESIAN_POINT('Ctrl Pts',(6.33961666743984,2.67292366620393,-1.83922581072696));
#6325=CARTESIAN_POINT('Ctrl Pts',(6.31780615152264,2.44050506298458,-2.13804674109713));
#6326=CARTESIAN_POINT('Ctrl Pts',(6.2714059908784,1.88503243339425,-2.64046788075814));
#6327=CARTESIAN_POINT('Ctrl Pts',(6.24713933049822,1.5668828873788,-2.84081655445888));
#6328=CARTESIAN_POINT('Ctrl Pts',(6.19758651601615,0.833882651370035,-3.14106384120585));
#6329=CARTESIAN_POINT('Ctrl Pts',(6.17379138942913,0.418933793946893,-3.22275679842899));
#6330=CARTESIAN_POINT('Ctrl Pts',(6.12215191209933,-0.419030059540087,-3.22274320089827));
#6331=CARTESIAN_POINT('Ctrl Pts',(6.094712349947,-0.8339727439216,-3.14104141762933));
#6332=CARTESIAN_POINT('Ctrl Pts',(6.04627022633677,-1.56696989769217,-2.84076801434325));
#6333=CARTESIAN_POINT('Ctrl Pts',(6.02479490891982,-1.8850989876462,-2.64041585876965));
#6334=CARTESIAN_POINT('Ctrl Pts',(5.97882691409565,-2.44053597286598,-2.13801055040736));
#6335=CARTESIAN_POINT('Ctrl Pts',(5.95462662454257,-2.67293699071203,-1.83920062617829));
#6336=CARTESIAN_POINT('Ctrl Pts',(5.93143566914408,-2.84862442585766,-1.5071351773836));
#6337=CARTESIAN_POINT('Origin',(13.3346225254169,0.,0.));
#6338=CARTESIAN_POINT('Ctrl Pts',(6.98780938168963,-2.84862442585767,1.50713517738359));
#6339=CARTESIAN_POINT('Ctrl Pts',(6.96461673398571,-2.67292417033464,1.83922485787345));
#6340=CARTESIAN_POINT('Ctrl Pts',(6.94280780367345,-2.44050636590057,2.13804508522705));
#6341=CARTESIAN_POINT('Ctrl Pts',(6.89641045018583,-1.88503543074861,2.64046564385251));
#6342=CARTESIAN_POINT('Ctrl Pts',(6.87214490040623,-1.56688677260614,2.8408143103698));
#6343=CARTESIAN_POINT('Ctrl Pts',(6.82259200319984,-0.833886022336899,3.14106319316094));
#6344=CARTESIAN_POINT('Ctrl Pts',(6.79879580149973,-0.418935352303087,3.22275683129305));
#6345=CARTESIAN_POINT('Ctrl Pts',(6.74715568383361,0.419032109002962,3.22274316802727));
#6346=CARTESIAN_POINT('Ctrl Pts',(6.71971658038225,0.833976594138993,3.14104064336343));
#6347=CARTESIAN_POINT('Ctrl Pts',(6.67127446793275,1.56697421210196,2.8407655317672));
#6348=CARTESIAN_POINT('Ctrl Pts',(6.64979841588627,1.88510230433969,2.64041337268491));
#6349=CARTESIAN_POINT('Ctrl Pts',(6.60382821780123,2.44053733263286,2.13800880301029));
#6350=CARTESIAN_POINT('Ctrl Pts',(6.5796265570515,2.67293750200331,1.83919965979063));
#6351=CARTESIAN_POINT('Ctrl Pts',(6.55643566914408,2.84862442585766,1.50713517738361));
#6352=CARTESIAN_POINT('Ctrl Pts',(6.74126248314343,-2.84862442585767,1.50713517738358));
#6353=CARTESIAN_POINT('Ctrl Pts',(6.71807147903754,-2.67293662172001,1.83920132360723));
#6354=CARTESIAN_POINT('Ctrl Pts',(6.69387220109966,-2.44053499142467,2.13801181152265));
#6355=CARTESIAN_POINT('Ctrl Pts',(6.64790581684408,-1.88509657801398,2.64041766749011));
#6356=CARTESIAN_POINT('Ctrl Pts',(6.62643102697238,-1.56696674689992,2.84076982924885));
#6357=CARTESIAN_POINT('Ctrl Pts',(6.57798886766466,-0.83396994252103,3.14104197668097));
#6358=CARTESIAN_POINT('Ctrl Pts',(6.55054895791701,-0.419028600918373,3.22274321667877));
#6359=CARTESIAN_POINT('Ctrl Pts',(6.49890995808951,0.418932567083949,3.22275678265165));
#6360=CARTESIAN_POINT('Ctrl Pts',(6.47511563910009,0.83388007696913,3.14106434094526));
#6361=CARTESIAN_POINT('Ctrl Pts',(6.42556291388709,1.56687996002487,2.84081824766148));
#6362=CARTESIAN_POINT('Ctrl Pts',(6.40129544396981,1.88503019047376,2.64046955776594));
#6363=CARTESIAN_POINT('Ctrl Pts',(6.35489322120279,2.440504096751,2.13804796912395));
#6364=CARTESIAN_POINT('Ctrl Pts',(6.3330815341862,2.67292329243067,1.83922651719288));
#6365=CARTESIAN_POINT('Ctrl Pts',(6.30988877059789,2.84862442585766,1.5071351773836));
#6366=CARTESIAN_POINT('Origin',(13.3346225254169,0.,0.));
#6367=CARTESIAN_POINT('Ctrl Pts',(7.36626248314343,2.84862442585767,-1.50713517738359));
#6368=CARTESIAN_POINT('Ctrl Pts',(7.34307154845362,2.67293714759447,-1.83920032965602));
#6369=CARTESIAN_POINT('Ctrl Pts',(7.31887085033888,2.44053638999056,-2.13801001440507));
#6370=CARTESIAN_POINT('Ctrl Pts',(7.27290220158661,1.88510000947698,-2.6404150921263));
#6371=CARTESIAN_POINT('Ctrl Pts',(7.25142666779954,1.56697123154665,-2.840767246207));
#6372=CARTESIAN_POINT('Ctrl Pts',(7.20298455318012,0.833973955625731,-3.14104117019823));
#6373=CARTESIAN_POINT('Ctrl Pts',(7.17554512945744,0.419030733458136,-3.22274318321347));
#6374=CARTESIAN_POINT('Ctrl Pts',(7.1239054598541,-0.41893420096316,-3.22275681610992));
#6375=CARTESIAN_POINT('Ctrl Pts',(7.1001100099163,-0.833883603332628,-3.14106366248313));
#6376=CARTESIAN_POINT('Ctrl Pts',(7.05055716572934,-1.56688400609692,-2.84081590809281));
#6377=CARTESIAN_POINT('Ctrl Pts',(7.02629083440148,-1.88503329554496,-2.64046723723885));
#6378=CARTESIAN_POINT('Ctrl Pts',(6.97989150871425,-2.44050543797639,-2.1380462647074));
#6379=CARTESIAN_POINT('Ctrl Pts',(6.95808146568176,-2.67292381139898,-1.83922553629492));
#6380=CARTESIAN_POINT('Ctrl Pts',(6.93488877059789,-2.84862442585766,-1.50713517738361));
#6381=CARTESIAN_POINT('Ctrl Pts',(7.61280938168963,2.84862442585767,-1.50713517738358));
#6382=CARTESIAN_POINT('Ctrl Pts',(7.58961679791791,2.67292465466507,-1.83922394244429));
#6383=CARTESIAN_POINT('Ctrl Pts',(7.56780937603312,2.4405076176909,-2.13804349415313));
#6384=CARTESIAN_POINT('Ctrl Pts',(7.52141471022063,1.88503828547658,-2.64046351751637));
#6385=CARTESIAN_POINT('Ctrl Pts',(7.49715023346056,1.5668904458648,-2.84081219200252));
#6386=CARTESIAN_POINT('Ctrl Pts',(7.44759729996001,0.83388918910371,-3.14106258507959));
#6387=CARTESIAN_POINT('Ctrl Pts',(7.42380009623393,0.418936811450608,-3.2227568633683));
#6388=CARTESIAN_POINT('Ctrl Pts',(7.37215937688665,-0.419034049172175,-3.22274313594519));
#6389=CARTESIAN_POINT('Ctrl Pts',(7.34472069647923,-0.833980230161243,-3.14103991147119));
#6390=CARTESIAN_POINT('Ctrl Pts',(7.29627855235602,-1.56697830211052,-2.84076318151702));
#6391=CARTESIAN_POINT('Ctrl Pts',(7.27480177875458,-1.88510546907338,-2.64041100465428));
#6392=CARTESIAN_POINT('Ctrl Pts',(7.22882945925579,-2.4405386406335,-2.13800712195888));
#6393=CARTESIAN_POINT('Ctrl Pts',(7.20462649212882,-2.67293799383723,-1.83919873017917));
#6394=CARTESIAN_POINT('Ctrl Pts',(7.18143566914407,-2.84862442585766,-1.5071351773836));
#6395=CARTESIAN_POINT('Origin',(13.3346225254169,0.,0.));
#6396=CARTESIAN_POINT('Ctrl Pts',(8.23780938168964,-2.84862442585767,1.50713517738359));
#6397=CARTESIAN_POINT('Ctrl Pts',(8.21461685940783,-2.67292512049342,1.83922306198576));
#6398=CARTESIAN_POINT('Ctrl Pts',(8.19281087455296,-2.44050882170521,2.13804196363864));
#6399=CARTESIAN_POINT('Ctrl Pts',(8.1464187852286,-1.88504100812479,2.64046149341013));
#6400=CARTESIAN_POINT('Ctrl Pts',(8.12215534609299,-1.56689392390231,2.8408101893104));
#6401=CARTESIAN_POINT('Ctrl Pts',(8.07260241763158,-0.833892168503167,3.14106201364612));
#6402=CARTESIAN_POINT('Ctrl Pts',(8.04880427870365,-0.418938179713951,3.22275689468293));
#6403=CARTESIAN_POINT('Ctrl Pts',(7.99716299314995,0.419035888601267,3.22274310462381));
#6404=CARTESIAN_POINT('Ctrl Pts',(7.96972470330544,0.833983669061916,3.14103921859861));
#6405=CARTESIAN_POINT('Ctrl Pts',(7.92128248949699,1.56698218507457,2.84076095324196));
#6406=CARTESIAN_POINT('Ctrl Pts',(7.89980500730298,1.88510849285657,2.64040874595429));
#6407=CARTESIAN_POINT('Ctrl Pts',(7.85383064307685,2.44053990018433,2.13800550301122));
#6408=CARTESIAN_POINT('Ctrl Pts',(7.82962642961006,2.67293846745991,1.83919783498865));
#6409=CARTESIAN_POINT('Ctrl Pts',(7.80643566914408,2.84862442585766,1.50713517738361));
#6410=CARTESIAN_POINT('Ctrl Pts',(7.99126248314343,-2.84862442585768,1.50713517738358));
#6411=CARTESIAN_POINT('Ctrl Pts',(7.96807161517476,-2.67293765305305,1.8391993742927));
#6412=CARTESIAN_POINT('Ctrl Pts',(7.94386956540416,-2.44053773423915,2.13800828689579));
#6413=CARTESIAN_POINT('Ctrl Pts',(7.8978987379663,-1.88510328046092,2.64041264157304));
#6414=CARTESIAN_POINT('Ctrl Pts',(7.87642247339536,-1.56697547832239,2.84076480352758));
#6415=CARTESIAN_POINT('Ctrl Pts',(7.82798035683828,-0.833977741266314,3.1410404086955));
#6416=CARTESIAN_POINT('Ctrl Pts',(7.80054138100634,-0.419032750058116,3.22274315055883));
#6417=CARTESIAN_POINT('Ctrl Pts',(7.74890108275571,0.41893572916163,3.22275684875764));
#6418=CARTESIAN_POINT('Ctrl Pts',(7.72510457983489,0.833886912410527,3.14106302656229));
#6419=CARTESIAN_POINT('Ctrl Pts',(7.67555166710805,1.56688782720213,2.84081370204725));
#6420=CARTESIAN_POINT('Ctrl Pts',(7.65128643511704,1.88503624982873,2.6404650337404));
#6421=CARTESIAN_POINT('Ctrl Pts',(7.60488988062576,2.4405067254997,2.1380446283454));
#6422=CARTESIAN_POINT('Ctrl Pts',(7.58308139992277,2.67292430956845,1.83922459470871));
#6423=CARTESIAN_POINT('Ctrl Pts',(7.55988877059788,2.84862442585767,1.5071351773836));
#6424=CARTESIAN_POINT('Origin',(13.3346225254169,0.,0.));
#6425=CARTESIAN_POINT('Ctrl Pts',(8.61626248314342,2.84862442585767,-1.50713517738359));
#6426=CARTESIAN_POINT('Ctrl Pts',(8.59307167937735,2.6729381394319,-1.83919845499182));
#6427=CARTESIAN_POINT('Ctrl Pts',(8.56886834131465,2.4405390277266,-2.13800662444666));
#6428=CARTESIAN_POINT('Ctrl Pts',(8.52289541547226,1.88510640283117,-2.64041030642139));
#6429=CARTESIAN_POINT('Ctrl Pts',(8.5014184331626,1.56697950597947,-2.84076249002305));
#6430=CARTESIAN_POINT('Ctrl Pts',(8.4529762733107,0.833981317909065,-3.14103968854607));
#6431=CARTESIAN_POINT('Ctrl Pts',(8.42553771068221,0.419034659963695,-3.22274311868561));
#6432=CARTESIAN_POINT('Ctrl Pts',(8.37389682146955,-0.418937160698148,-3.22275688062404));
#6433=CARTESIAN_POINT('Ctrl Pts',(8.3500993367416,-0.833890022429059,-3.14106242959182));
#6434=CARTESIAN_POINT('Ctrl Pts',(8.30054640034428,-1.56689144144792,-2.840811618658));
#6435=CARTESIAN_POINT('Ctrl Pts',(8.27628223077126,-1.88503906470035,-2.64046293826904));
#6436=CARTESIAN_POINT('Ctrl Pts',(8.22988833051641,-2.44050796291601,-2.13804305549113));
#6437=CARTESIAN_POINT('Ctrl Pts',(8.20808133672534,-2.67292478833241,-1.83922368980068));
#6438=CARTESIAN_POINT('Ctrl Pts',(8.18488877059787,-2.84862442585766,-1.50713517738361));
#6439=CARTESIAN_POINT('Ctrl Pts',(8.86280938168963,2.84862442585767,-1.50713517738358));
#6440=CARTESIAN_POINT('Ctrl Pts',(8.83961691861088,2.67292556899732,-1.83922221427203));
#6441=CARTESIAN_POINT('Ctrl Pts',(8.81781230459156,2.44050998098217,-2.1380404898397));
#6442=CARTESIAN_POINT('Ctrl Pts',(8.77142268806627,1.88504360819397,-2.64045956402922));
#6443=CARTESIAN_POINT('Ctrl Pts',(8.74716025315798,1.5668972217526,-2.84080829327991));
#6444=CARTESIAN_POINT('Ctrl Pts',(8.69760736655834,0.833894975613833,-3.14106147589125));
#6445=CARTESIAN_POINT('Ctrl Pts',(8.67380835365215,0.418939464544131,-3.22275692526376));
#6446=CARTESIAN_POINT('Ctrl Pts',(8.62216653451732,-0.419037634971519,-3.22274307403636));
#6447=CARTESIAN_POINT('Ctrl Pts',(8.59472860558992,-0.833986926159643,-3.14103856173539));
#6448=CARTESIAN_POINT('Ctrl Pts',(8.54628628834907,-1.56698587659116,-2.84075883764607));
#6449=CARTESIAN_POINT('Ctrl Pts',(8.52480811038229,-1.88511138561726,-2.64040658872676));
#6450=CARTESIAN_POINT('Ctrl Pts',(8.47883177342321,-2.44054111429785,-2.13800394231365));
#6451=CARTESIAN_POINT('Ctrl Pts',(8.45462636934577,-2.67293892400329,-1.83919697207958));
#6452=CARTESIAN_POINT('Ctrl Pts',(8.43143566914408,-2.84862442585767,-1.5071351773836));
#6453=CARTESIAN_POINT('Origin',(13.3346225254169,0.,0.));
#6454=CARTESIAN_POINT('Ctrl Pts',(9.48780938168962,-2.84862442585767,1.50713517738359));
#6455=CARTESIAN_POINT('Ctrl Pts',(9.4646169756685,-2.67292600124808,1.83922139727825));
#6456=CARTESIAN_POINT('Ctrl Pts',(9.44281367098766,-2.44051109828623,2.1380390692589));
#6457=CARTESIAN_POINT('Ctrl Pts',(9.39642643037003,-1.88504609426699,2.64045772260141));
#6458=CARTESIAN_POINT('Ctrl Pts',(9.37216496812315,-1.56690035294904,2.84080649580198));
#6459=CARTESIAN_POINT('Ctrl Pts',(9.32261215620681,-0.833897623979761,3.14106096914872));
#6460=CARTESIAN_POINT('Ctrl Pts',(9.29881232552417,-0.418940672627908,3.22275695513633));
#6461=CARTESIAN_POINT('Ctrl Pts',(9.24717000287363,0.419039295201162,3.22274304415726));
#6462=CARTESIAN_POINT('Ctrl Pts',(9.21973240775526,0.833990015237942,3.14103793817188));
#6463=CARTESIAN_POINT('Ctrl Pts',(9.17128995711388,1.56698939071643,2.84075682635676));
#6464=CARTESIAN_POINT('Ctrl Pts',(9.14981109602737,1.88511415633464,2.64040452587235));
#6465=CARTESIAN_POINT('Ctrl Pts',(9.10383285405132,2.44054228571856,2.13800243635496));
#6466=CARTESIAN_POINT('Ctrl Pts',(9.07962631119985,2.67293936449861,1.83919613950281));
#6467=CARTESIAN_POINT('Ctrl Pts',(9.05643566914408,2.84862442585766,1.50713517738361));
#6468=CARTESIAN_POINT('Ctrl Pts',(9.24126248314343,-2.84862442585767,1.50713517738359));
#6469=CARTESIAN_POINT('Ctrl Pts',(9.21807174122128,-2.67293860794215,1.83919756946426));
#6470=CARTESIAN_POINT('Ctrl Pts',(9.19386717359377,-2.44054027367612,2.13800502293484));
#6471=CARTESIAN_POINT('Ctrl Pts',(9.14789222461089,-1.88510938726485,2.64040807821378));
#6472=CARTESIAN_POINT('Ctrl Pts',(9.12641453748589,-1.56698333133364,2.84076029566696));
#6473=CARTESIAN_POINT('Ctrl Pts',(9.07797229763274,-0.833984702087806,3.14103900650164));
#6474=CARTESIAN_POINT('Ctrl Pts',(9.05053411659157,-0.419036471460086,3.22274308756608));
#6475=CARTESIAN_POINT('Ctrl Pts',(8.99889267102348,0.418938503628748,3.22275691173686));
#6476=CARTESIAN_POINT('Ctrl Pts',(8.97509426960511,0.833892949681618,3.14106186836253));
#6477=CARTESIAN_POINT('Ctrl Pts',(8.92554134949045,1.56689486505516,2.84080964819597));
#6478=CARTESIAN_POINT('Ctrl Pts',(8.90127820754495,1.88504175038528,2.64046094274164));
#6479=CARTESIAN_POINT('Ctrl Pts',(8.85488685261699,2.44050915347968,2.13804154202824));
#6480=CARTESIAN_POINT('Ctrl Pts',(8.83308127592298,2.67292524895216,1.83922281918689));
#6481=CARTESIAN_POINT('Ctrl Pts',(8.80988877059788,2.84862442585767,1.50713517738359));
#6482=CARTESIAN_POINT('Origin',(13.3346225254169,0.,0.));
#6483=CARTESIAN_POINT('Ctrl Pts',(9.86626248314343,2.84862442585767,-1.50713517738359));
#6484=CARTESIAN_POINT('Ctrl Pts',(9.84307180085188,2.67293905968497,-1.83919671562868));
#6485=CARTESIAN_POINT('Ctrl Pts',(9.81886605820617,2.44054147501838,-2.13800347861122));
#6486=CARTESIAN_POINT('Ctrl Pts',(9.77288915678148,1.88511224339947,-2.64040594932443));
#6487=CARTESIAN_POINT('Ctrl Pts',(9.75141077761425,1.56698696950969,-2.84075821144642));
#6488=CARTESIAN_POINT('Ctrl Pts',(9.70296842516841,0.833987908650847,-3.14103835964394));
#6489=CARTESIAN_POINT('Ctrl Pts',(9.67553059684219,0.419038191995453,-3.22274305717364));
#6490=CARTESIAN_POINT('Ctrl Pts',(9.62388862676483,-0.418939765168384,-3.22275694212268));
#6491=CARTESIAN_POINT('Ctrl Pts',(9.60008936835002,-0.833895708774181,-3.14106133999854));
#6492=CARTESIAN_POINT('Ctrl Pts',(9.55053650011739,-1.56689811259611,-2.84080778192593));
#6493=CARTESIAN_POINT('Ctrl Pts',(9.52627435295588,-1.88504431610193,-2.64045903987891));
#6494=CARTESIAN_POINT('Ctrl Pts',(9.47988544172846,-2.44051030014507,-2.13804008421938));
#6495=CARTESIAN_POINT('Ctrl Pts',(9.45808121736454,-2.67292569257261,-1.83922198070335));
#6496=CARTESIAN_POINT('Ctrl Pts',(9.43488877059788,-2.84862442585766,-1.5071351773836));
#6497=CARTESIAN_POINT('Ctrl Pts',(10.1128093816896,2.84862442585767,-1.50713517738358));
#6498=CARTESIAN_POINT('Ctrl Pts',(10.0896170307097,2.67292641822307,-1.83922060915709));
#6499=CARTESIAN_POINT('Ctrl Pts',(10.0678149781225,2.44051217613953,-2.13803769870501));
#6500=CARTESIAN_POINT('Ctrl Pts',(10.021430022701,1.88504847411913,-2.64045596299845));
#6501=CARTESIAN_POINT('Ctrl Pts',(9.99716950323258,1.56690332970733,-2.84080478956146));
#6502=CARTESIAN_POINT('Ctrl Pts',(9.94761679526431,0.833900125799363,-3.1410604910179));
#6503=CARTESIAN_POINT('Ctrl Pts',(9.92381619849262,0.418941809982594,-3.222756984325));
#6504=CARTESIAN_POINT('Ctrl Pts',(9.87217340008585,-0.419040875537337,-3.22274301496216));
#6505=CARTESIAN_POINT('Ctrl Pts',(9.84473611394561,-0.8339929487316,-3.14103734546267));
#6506=CARTESIAN_POINT('Ctrl Pts',(9.79629350329155,-1.56699274015167,-2.840754911813));
#6507=CARTESIAN_POINT('Ctrl Pts',(9.77481397155242,-1.88511681315177,-2.64040255095991));
#6508=CARTESIAN_POINT('Ctrl Pts',(9.72883388836341,-2.44054341695358,-2.13800098192721));
#6509=CARTESIAN_POINT('Ctrl Pts',(9.70462625504794,-2.67293978988799,-1.83919533547766));
#6510=CARTESIAN_POINT('Ctrl Pts',(9.68143566914409,-2.84862442585767,-1.50713517738359));
#6511=CARTESIAN_POINT('Origin',(13.3346225254169,0.,0.));
#6512=CARTESIAN_POINT('Ctrl Pts',(10.7378093816897,-2.84862442585767,1.50713517738359));
#6513=CARTESIAN_POINT('Ctrl Pts',(10.7146170838525,-2.67292682081615,1.83921984821904));
#6514=CARTESIAN_POINT('Ctrl Pts',(10.6928162299734,-2.44051321684886,2.13803637525888));
#6515=CARTESIAN_POINT('Ctrl Pts',(10.6464334746689,-1.88505075481185,2.64045427966082));
#6516=CARTESIAN_POINT('Ctrl Pts',(10.6221738696468,-1.56690616308131,2.84080316794297));
#6517=CARTESIAN_POINT('Ctrl Pts',(10.5726212917232,-0.833902492085885,3.14106003933216));
#6518=CARTESIAN_POINT('Ctrl Pts',(10.5488199764818,-0.418942882035734,3.22275701285304));
#6519=CARTESIAN_POINT('Ctrl Pts',(10.497176727996,0.41904238163632,3.2227429864278));
#6520=CARTESIAN_POINT('Ctrl Pts',(10.4697397280512,0.833995737887798,3.14103678139506));
#6521=CARTESIAN_POINT('Ctrl Pts',(10.4212969337585,1.56699593640378,2.84075308716898));
#6522=CARTESIAN_POINT('Ctrl Pts',(10.3998167436331,1.88511936347304,2.64040065814822));
#6523=CARTESIAN_POINT('Ctrl Pts',(10.3538348794489,2.44054451029931,2.13799957609175));
#6524=CARTESIAN_POINT('Ctrl Pts',(10.3296262007761,2.67294020103435,1.83919455837315));
#6525=CARTESIAN_POINT('Ctrl Pts',(10.3064356691441,2.84862442585766,1.50713517738361));
#6526=CARTESIAN_POINT('Ctrl Pts',(10.4912624831434,-2.84862442585767,1.50713517738358));
#6527=CARTESIAN_POINT('Ctrl Pts',(10.4680718584017,-2.67293949566439,1.8391958915874));
#6528=CARTESIAN_POINT('Ctrl Pts',(10.443864991504,-2.44054263442528,2.13800198805734));
#6529=CARTESIAN_POINT('Ctrl Pts',(10.3978862041699,-1.88511497995812,2.6404039128587));
#6530=CARTESIAN_POINT('Ctrl Pts',(10.3764071455606,-1.56699043414843,2.84075622923762));
#6531=CARTESIAN_POINT('Ctrl Pts',(10.3279646515796,-0.833990950968164,3.14103774534431));
#6532=CARTESIAN_POINT('Ctrl Pts',(10.3005271495537,-0.419039828282384,3.22274302748307));
#6533=CARTESIAN_POINT('Ctrl Pts',(10.2488846843312,0.418940951798243,3.22275697180674));
#6534=CARTESIAN_POINT('Ctrl Pts',(10.225084623748,0.833898312837746,3.14106084191516));
#6535=CARTESIAN_POINT('Ctrl Pts',(10.1755318391322,1.56690119719985,2.84080601198241));
#6536=CARTESIAN_POINT('Ctrl Pts',(10.1512706556972,1.88504677018556,2.64045722310611));
#6537=CARTESIAN_POINT('Ctrl Pts',(10.1048840931523,2.44051140560248,2.13803867866086));
#6538=CARTESIAN_POINT('Ctrl Pts',(10.0830811609124,2.67292612023633,1.83922117237949));
#6539=CARTESIAN_POINT('Ctrl Pts',(10.0598887705979,2.84862442585767,1.50713517738359));
#6540=CARTESIAN_POINT('Origin',(13.3346225254169,0.,0.));
#6541=CARTESIAN_POINT('',(11.0234525205638,1.87154958983019,-2.62278522261047));
#6542=CARTESIAN_POINT('Ctrl Pts',(11.0230520901771,1.87192183080106,-2.62336162620986));
#6543=CARTESIAN_POINT('Ctrl Pts',(11.0079418888754,1.66946798355985,-2.76782427771551));
#6544=CARTESIAN_POINT('Ctrl Pts',(10.9932884442656,1.45097662306557,-2.88836270650252));
#6545=CARTESIAN_POINT('Ctrl Pts',(10.9632934504298,0.991158559414914,-3.07657202253502));
#6546=CARTESIAN_POINT('Ctrl Pts',(10.9476487851673,0.751458310552837,-3.14371789775113));
#6547=CARTESIAN_POINT('Ctrl Pts',(10.905150297864,0.0912513489784357,-3.24878003151173));
#6548=CARTESIAN_POINT('Ctrl Pts',(10.8795320204101,-0.332960972250965,-3.232971873478));
#6549=CARTESIAN_POINT('Ctrl Pts',(10.8417942436161,-0.945997583469522,-3.08789051095225));
#6550=CARTESIAN_POINT('Ctrl Pts',(10.8292395318735,-1.14458398877081,-3.01991762265664));
#6551=CARTESIAN_POINT('Ctrl Pts',(10.7939402148955,-1.65629153641311,-2.7869856969747));
#6552=CARTESIAN_POINT('Ctrl Pts',(10.7711998614304,-1.95124147240243,-2.58907215729383));
#6553=CARTESIAN_POINT('Ctrl Pts',(10.7274837181104,-2.46648776794441,-2.10434252694404));
#6554=CARTESIAN_POINT('Ctrl Pts',(10.7067726755519,-2.68283879666383,-1.82048530009627));
#6555=CARTESIAN_POINT('Ctrl Pts',(10.6848887705979,-2.84862442585766,-1.5071351773836));
#6556=CARTESIAN_POINT('',(11.0238490761438,-1.87158653173898,-2.62360084935061));
#6557=CARTESIAN_POINT('Origin',(11.0238490761438,0.,0.));
#6558=CARTESIAN_POINT('Ctrl Pts',(11.0238490761438,-1.87158653173898,-2.62360084935061));
#6559=CARTESIAN_POINT('Ctrl Pts',(11.0084296939351,-2.07493204384538,-2.4785411609296));
#6560=CARTESIAN_POINT('Ctrl Pts',(10.99328545226,-2.26072639839162,-2.31033087287213));
#6561=CARTESIAN_POINT('Ctrl Pts',(10.962448845779,-2.58972688979184,-1.934380324523));
#6562=CARTESIAN_POINT('Ctrl Pts',(10.9468549948036,-2.7318124303945,-1.72792061753715));
#6563=CARTESIAN_POINT('Ctrl Pts',(10.9314356691441,-2.84862442585767,-1.5071351773836));
#6564=CARTESIAN_POINT('Ctrl Pts',(11.1008112312664,1.68942544263115,3.40346056344526));
#6565=CARTESIAN_POINT('Ctrl Pts',(11.0751571795589,2.12830620414844,3.18560690803575));
#6566=CARTESIAN_POINT('Ctrl Pts',(11.0495031278513,2.52436782889846,2.88189967479167));
#6567=CARTESIAN_POINT('Ctrl Pts',(11.0238490761438,2.84862442585767,2.51456577037539));
#6568=CARTESIAN_POINT('Ctrl Pts',(11.0751571795589,1.70918178686444,3.44326104044715));
#6569=CARTESIAN_POINT('Ctrl Pts',(11.0495031278513,2.15319487277031,3.22285977820035));
#6570=CARTESIAN_POINT('Ctrl Pts',(11.0238490761438,2.55388808977572,2.91560095605822));
#6571=CARTESIAN_POINT('Ctrl Pts',(10.9981950244362,2.88193658236276,2.54397140480186));
#6572=CARTESIAN_POINT('Ctrl Pts',(11.0495031278513,1.72893813109773,3.48306151744904));
#6573=CARTESIAN_POINT('Ctrl Pts',(11.0238490761438,2.17808354139218,3.26011264836494));
#6574=CARTESIAN_POINT('Ctrl Pts',(10.9981950244362,2.58340835065299,2.94930223732478));
#6575=CARTESIAN_POINT('Ctrl Pts',(10.9725409727286,2.91524873886784,2.57337703922832));
#6576=CARTESIAN_POINT('Ctrl Pts',(11.0238490761438,1.74869447533101,3.52286199445093));
#6577=CARTESIAN_POINT('Ctrl Pts',(10.9981950244362,2.20297221001404,3.29736551852953));
#6578=CARTESIAN_POINT('Ctrl Pts',(10.9725409727286,2.61292861153025,2.98300351859134));
#6579=CARTESIAN_POINT('Ctrl Pts',(10.9468869210211,2.94856089537293,2.60278267365479));
#6580=CARTESIAN_POINT('',(11.0238490761438,1.74869447533103,3.52286199445092));
#6581=CARTESIAN_POINT('Ctrl Pts',(11.0238490761438,1.74869447533103,3.52286199445092));
#6582=CARTESIAN_POINT('Ctrl Pts',(11.0006887763626,2.15881326042978,3.31928534147352));
#6583=CARTESIAN_POINT('Ctrl Pts',(10.9775284765815,2.53280859423868,3.0432801490367));
#6584=CARTESIAN_POINT('Ctrl Pts',(10.9543681768003,2.84860418144656,2.71177492056083));
#6585=CARTESIAN_POINT('Origin',(11.0238490761448,0.32028972767158,0.987026521741422));
#6586=CARTESIAN_POINT('Ctrl Pts',(3.61729894227909,2.84735487989943,-1.50582500201333));
#6587=CARTESIAN_POINT('Ctrl Pts',(3.56935691049898,2.48448123509701,-2.19199227724466));
#6588=CARTESIAN_POINT('Ctrl Pts',(3.47348446621381,1.24430262445242,-3.28807336521129));
#6589=CARTESIAN_POINT('Ctrl Pts',(3.32966999014855,-1.2443026244524,-3.28807336521131));
#6590=CARTESIAN_POINT('Ctrl Pts',(3.23379754586339,-2.484481235097,-2.19199227724467));
#6591=CARTESIAN_POINT('Ctrl Pts',(3.18585551408329,-2.84735487989942,-1.50582500201335));
#6592=CARTESIAN_POINT('Ctrl Pts',(3.48027739894494,3.0571514143775,-1.6167760004937));
#6593=CARTESIAN_POINT('Ctrl Pts',(3.43233536716482,2.66754080269033,-2.35350090639904));
#6594=CARTESIAN_POINT('Ctrl Pts',(3.33646292287966,1.33598433939948,-3.53034256811279));
#6595=CARTESIAN_POINT('Ctrl Pts',(3.1926484468144,-1.33598433939945,-3.53034256811281));
#6596=CARTESIAN_POINT('Ctrl Pts',(3.09677600252924,-2.66754080269031,-2.35350090639906));
#6597=CARTESIAN_POINT('Ctrl Pts',(3.04883397074914,-3.05715141437748,-1.61677600049373));
#6598=CARTESIAN_POINT('Ctrl Pts',(3.34325585561077,3.26694794885555,-1.72772699897407));
#6599=CARTESIAN_POINT('Ctrl Pts',(3.29531382383067,2.85060037028365,-2.5150095355534));
#6600=CARTESIAN_POINT('Ctrl Pts',(3.19944137954551,1.42766605434656,-3.7726117710143));
#6601=CARTESIAN_POINT('Ctrl Pts',(3.05562690348025,-1.42766605434652,-3.77261177101431));
#6602=CARTESIAN_POINT('Ctrl Pts',(2.95975445919508,-2.85060037028362,-2.51500953555344));
#6603=CARTESIAN_POINT('Ctrl Pts',(2.91181242741498,-3.26694794885553,-1.7277269989741));
#6604=CARTESIAN_POINT('Ctrl Pts',(3.20623431227662,3.47674448333362,-1.83867799745444));
#6605=CARTESIAN_POINT('Ctrl Pts',(3.15829228049652,3.03365993787697,-2.67651816470778));
#6606=CARTESIAN_POINT('Ctrl Pts',(3.06241983621135,1.51934776929363,-4.01488097391579));
#6607=CARTESIAN_POINT('Ctrl Pts',(2.91860536014609,-1.51934776929357,-4.01488097391582));
#6608=CARTESIAN_POINT('Ctrl Pts',(2.82273291586093,-3.03365993787694,-2.67651816470782));
#6609=CARTESIAN_POINT('Ctrl Pts',(2.77479088408083,-3.47674448333358,-1.83867799745449));
#6610=CARTESIAN_POINT('',(3.02384926683068,0.656743230768742,-3.87731376376925));
#6611=CARTESIAN_POINT('Ctrl Pts',(3.02384907614375,0.656739510617936,-3.8773143808427));
#6612=CARTESIAN_POINT('Ctrl Pts',(3.02384907614375,0.535250361064991,-3.88669383362235));
#6613=CARTESIAN_POINT('Ctrl Pts',(3.02384907614375,0.413571786056566,-3.89044850980063));
#6614=CARTESIAN_POINT('Ctrl Pts',(3.02384907614375,0.292110717075194,-3.8886442850087));
#6615=CARTESIAN_POINT('Ctrl Pts',(3.02384907614375,0.170355995076364,-3.88683569819313));
#6616=CARTESIAN_POINT('Ctrl Pts',(3.02384907614374,0.048818954209201,-3.87944114113221));
#6617=CARTESIAN_POINT('Ctrl Pts',(3.02384907614374,-0.0720841978754196,
-3.86647526034617));
#6618=CARTESIAN_POINT('Ctrl Pts',(3.02384907614375,-0.190730889068619,-3.85375136665815));
#6619=CARTESIAN_POINT('Ctrl Pts',(3.02384907614375,-0.308767876865074,-3.83566186702548));
#6620=CARTESIAN_POINT('Ctrl Pts',(3.02384907614376,-0.425783805159,-3.81217453465478));
#6621=CARTESIAN_POINT('Ctrl Pts',(3.02384907614375,-0.503663329837124,-3.79654262618167));
#6622=CARTESIAN_POINT('Ctrl Pts',(3.02384907614375,-0.581090187929004,-3.77851880324373));
#6623=CARTESIAN_POINT('Ctrl Pts',(3.02384907614375,-0.657936143484074,-3.75808285085038));
#6624=CARTESIAN_POINT('Ctrl Pts',(3.02384907614375,-0.701243993343972,-3.74656582107826));
#6625=CARTESIAN_POINT('Ctrl Pts',(3.02384907614375,-0.744367230920925,-3.73428252775787));
#6626=CARTESIAN_POINT('Ctrl Pts',(3.02384907614375,-0.787281908740254,-3.72122819370286));
#6627=CARTESIAN_POINT('Ctrl Pts',(3.02384907614375,-0.813645800332897,-3.71320848889955));
#6628=CARTESIAN_POINT('Ctrl Pts',(3.02384907614375,-0.839937635499688,-3.7048954060654));
#6629=CARTESIAN_POINT('Ctrl Pts',(3.02384907614375,-0.866109900983181,-3.69630194449922));
#6630=CARTESIAN_POINT('Ctrl Pts',(3.02384907614375,-0.977678019052361,-3.65966941319454));
#6631=CARTESIAN_POINT('Ctrl Pts',(3.02384907614375,-1.08720975521468,-3.61790757563285));
#6632=CARTESIAN_POINT('Ctrl Pts',(3.02384907614375,-1.1943262208367,-3.57102425033263));
#6633=CARTESIAN_POINT('Ctrl Pts',(3.02384907614375,-1.23891450694224,-3.55150860341573));
#6634=CARTESIAN_POINT('Ctrl Pts',(3.02384907614375,-1.28308403622502,-3.53110498594551));
#6635=CARTESIAN_POINT('Ctrl Pts',(3.02384907614375,-1.32680617741716,-3.50981161930699));
#6636=CARTESIAN_POINT('Ctrl Pts',(3.02384907614375,-1.43289130004467,-3.45814650526161));
#6637=CARTESIAN_POINT('Ctrl Pts',(3.02384907614375,-1.53634510039748,-3.40124585112717));
#6638=CARTESIAN_POINT('Ctrl Pts',(3.02384907614375,-1.6368809757992,-3.33940450460461));
#6639=CARTESIAN_POINT('Ctrl Pts',(3.02384907614375,-1.73706849226998,-3.27777743965345));
#6640=CARTESIAN_POINT('Ctrl Pts',(3.02384907614375,-1.83435879667051,-3.21124313841696));
#6641=CARTESIAN_POINT('Ctrl Pts',(3.02384907614375,-1.92842806804127,-3.14006162188339));
#6642=CARTESIAN_POINT('Ctrl Pts',(3.02384907614375,-1.98023292809871,-3.10086127038747));
#6643=CARTESIAN_POINT('Ctrl Pts',(3.02384907614375,-2.0310601552513,-3.06025100909125));
#6644=CARTESIAN_POINT('Ctrl Pts',(3.02384907614375,-2.0808495508829,-3.018271330865));
#6645=CARTESIAN_POINT('Ctrl Pts',(3.02384907614375,-2.10068222578663,-3.00154951088178));
#6646=CARTESIAN_POINT('Ctrl Pts',(3.02384907614375,-2.12033510199989,-2.98462300334751));
#6647=CARTESIAN_POINT('Ctrl Pts',(3.02384907614375,-2.13979707289648,-2.96750248510467));
#6648=CARTESIAN_POINT('Ctrl Pts',(3.02384907614375,-2.22653562887142,-2.89119936874417));
#6649=CARTESIAN_POINT('Ctrl Pts',(3.02384907614375,-2.30953913984263,-2.81099999949489));
#6650=CARTESIAN_POINT('Ctrl Pts',(3.02384907614375,-2.3885507954711,-2.72719596287315));
#6651=CARTESIAN_POINT('Ctrl Pts',(3.02384907614375,-2.46682747261444,-2.64417148419631));
#6652=CARTESIAN_POINT('Ctrl Pts',(3.02384907614375,-2.5411866444644,-2.55760835213176));
#6653=CARTESIAN_POINT('Ctrl Pts',(3.02384907614375,-2.61133671528648,-2.46776198450897));
#6654=CARTESIAN_POINT('Ctrl Pts',(3.02384907614375,-2.68107943019947,-2.37843734763188));
#6655=CARTESIAN_POINT('Ctrl Pts',(3.02384907614376,-2.7466622109697,-2.28586682986901));
#6656=CARTESIAN_POINT('Ctrl Pts',(3.02384907614376,-2.80775053351277,-2.19028389748535));
#6657=CARTESIAN_POINT('Ctrl Pts',(3.02384907614376,-2.82131446704314,-2.16906084719493));
#6658=CARTESIAN_POINT('Ctrl Pts',(3.02384907614375,-2.8346566170922,-2.14768923548601));
#6659=CARTESIAN_POINT('Ctrl Pts',(3.02384907614375,-2.84777296580223,-2.12617155036607));
#6660=CARTESIAN_POINT('Ctrl Pts',(3.15165719587644,2.84680317627431,-2.71057532546662));
#6661=CARTESIAN_POINT('Ctrl Pts',(3.12190753622973,2.44054601589642,-3.13625204053632));
#6662=CARTESIAN_POINT('Ctrl Pts',(3.07930489321447,1.72451193341724,-3.61812485237549));
#6663=CARTESIAN_POINT('Ctrl Pts',(3.03670225019923,0.907494732982598,-3.83572067768669));
#6664=CARTESIAN_POINT('Ctrl Pts',(3.02384926683068,0.656743230768742,-3.87731376376925));
#6665=CARTESIAN_POINT('Ctrl Pts',(4.86728743325252,2.84737399657633,-1.50583210302806));
#6666=CARTESIAN_POINT('Ctrl Pts',(4.81934534671256,2.48449826149224,-2.19200478877887));
#6667=CARTESIAN_POINT('Ctrl Pts',(4.72347284766753,1.24425292797664,-3.2880767251413));
#6668=CARTESIAN_POINT('Ctrl Pts',(4.57965826208255,-1.24425292797662,-3.28807672514131));
#6669=CARTESIAN_POINT('Ctrl Pts',(4.48378576303753,-2.48449826149223,-2.19200478877888));
#6670=CARTESIAN_POINT('Ctrl Pts',(4.43584367649757,-2.84737399657632,-1.50583210302808));
#6671=CARTESIAN_POINT('Ctrl Pts',(4.73026978102042,3.05716466492174,-1.61677977751342));
#6672=CARTESIAN_POINT('Ctrl Pts',(4.68232769448045,2.66755273603903,-2.35350873950932));
#6673=CARTESIAN_POINT('Ctrl Pts',(4.58645519543543,1.33592780232221,-3.53033777499559));
#6674=CARTESIAN_POINT('Ctrl Pts',(4.44264060985045,-1.33592780232218,-3.5303377749956));
#6675=CARTESIAN_POINT('Ctrl Pts',(4.34676811080543,-2.66755273603901,-2.35350873950934));
#6676=CARTESIAN_POINT('Ctrl Pts',(4.29882602426546,-3.05716466492172,-1.61677977751345));
#6677=CARTESIAN_POINT('Ctrl Pts',(4.5932521287883,3.26695533326716,-1.72772745199879));
#6678=CARTESIAN_POINT('Ctrl Pts',(4.54531004224834,2.85060721058582,-2.51501269023978));
#6679=CARTESIAN_POINT('Ctrl Pts',(4.44943754320332,1.42760267666778,-3.77259882484987));
#6680=CARTESIAN_POINT('Ctrl Pts',(4.30562295761834,-1.42760267666773,-3.77259882484989));
#6681=CARTESIAN_POINT('Ctrl Pts',(4.20975045857331,-2.85060721058579,-2.51501269023981));
#6682=CARTESIAN_POINT('Ctrl Pts',(4.16180837203335,-3.26695533326714,-1.72772745199882));
#6683=CARTESIAN_POINT('Ctrl Pts',(4.4562344765562,3.47674600161257,-1.83867512648414));
#6684=CARTESIAN_POINT('Ctrl Pts',(4.40829239001624,3.03366168513261,-2.67651664097024));
#6685=CARTESIAN_POINT('Ctrl Pts',(4.31241989097121,1.51927755101335,-4.01485987470417));
#6686=CARTESIAN_POINT('Ctrl Pts',(4.16860530538623,-1.5192775510133,-4.01485987470418));
#6687=CARTESIAN_POINT('Ctrl Pts',(4.07273280634121,-3.03366168513258,-2.67651664097028));
#6688=CARTESIAN_POINT('Ctrl Pts',(4.02479071980125,-3.47674600161254,-1.83867512648419));
#6689=CARTESIAN_POINT('Ctrl Pts',(4.40165719587644,2.84679199383306,-2.71057163545836));
#6690=CARTESIAN_POINT('Ctrl Pts',(4.37190753622973,2.44052493609236,-3.13624479621667));
#6691=CARTESIAN_POINT('Ctrl Pts',(4.29422746407797,1.13490282761621,-4.01485987470402));
#6692=CARTESIAN_POINT('Ctrl Pts',(4.18679773227948,-1.13490282761596,-4.01485987470424));
#6693=CARTESIAN_POINT('Ctrl Pts',(4.10911766012771,-2.44052493609232,-3.1362447962167));
#6694=CARTESIAN_POINT('Ctrl Pts',(4.079368000481,-2.84679199383302,-2.7105716354584));
#6695=CARTESIAN_POINT('Ctrl Pts',(6.11727672162286,2.84739173784017,-1.50583878760475));
#6696=CARTESIAN_POINT('Ctrl Pts',(6.06933458598282,2.48451405189022,-2.19201646962288));
#6697=CARTESIAN_POINT('Ctrl Pts',(5.97346203783771,1.2442095628356,-3.28807951087694));
#6698=CARTESIAN_POINT('Ctrl Pts',(5.82964735405254,-1.24420956283556,-3.28807951087695));
#6699=CARTESIAN_POINT('Ctrl Pts',(5.73377480590744,-2.48451405189019,-2.19201646962291));
#6700=CARTESIAN_POINT('Ctrl Pts',(5.68583267026739,-2.84739173784015,-1.50583878760479));
#6701=CARTESIAN_POINT('Ctrl Pts',(5.98026268903406,3.0571769462154,-1.61678337581823));
#6702=CARTESIAN_POINT('Ctrl Pts',(5.93232055339401,2.66756378514623,-2.35351607142707));
#6703=CARTESIAN_POINT('Ctrl Pts',(5.83644800524891,1.33587828510277,-3.53033295151763));
#6704=CARTESIAN_POINT('Ctrl Pts',(5.69263332146373,-1.33587828510273,-3.53033295151765));
#6705=CARTESIAN_POINT('Ctrl Pts',(5.59676077331864,-2.6675637851462,-2.35351607142711));
#6706=CARTESIAN_POINT('Ctrl Pts',(5.54881863767859,-3.05717694621537,-1.61678337581828));
#6707=CARTESIAN_POINT('Ctrl Pts',(5.84324865644526,3.26696215459064,-1.72772796403172));
#6708=CARTESIAN_POINT('Ctrl Pts',(5.79530652080522,2.85061351840224,-2.51501567323129));
#6709=CARTESIAN_POINT('Ctrl Pts',(5.69943397266011,1.42754700736996,-3.77258639215831));
#6710=CARTESIAN_POINT('Ctrl Pts',(5.55561928887494,-1.42754700736989,-3.77258639215833));
#6711=CARTESIAN_POINT('Ctrl Pts',(5.45974674072984,-2.8506135184022,-2.51501567323134));
#6712=CARTESIAN_POINT('Ctrl Pts',(5.41180460508979,-3.26696215459061,-1.72772796403177));
#6713=CARTESIAN_POINT('Ctrl Pts',(5.70623462385646,3.47674736296587,-1.8386725522452));
#6714=CARTESIAN_POINT('Ctrl Pts',(5.65829248821641,3.03366325165824,-2.67651527503548));
#6715=CARTESIAN_POINT('Ctrl Pts',(5.56241994007131,1.51921572963714,-4.01483983279899));
#6716=CARTESIAN_POINT('Ctrl Pts',(5.41860525628614,-1.51921572963706,-4.01483983279902));
#6717=CARTESIAN_POINT('Ctrl Pts',(5.32273270814104,-3.03366325165819,-2.67651527503554));
#6718=CARTESIAN_POINT('Ctrl Pts',(5.27479057250099,-3.47674736296583,-1.83867255224527));
#6719=CARTESIAN_POINT('Ctrl Pts',(5.65165719587644,2.8467821456932,-2.71056813036079));
#6720=CARTESIAN_POINT('Ctrl Pts',(5.62190753622973,2.44050637155411,-3.13623791491845));
#6721=CARTESIAN_POINT('Ctrl Pts',(5.54422746407797,1.13485587203874,-4.01483983279886));
#6722=CARTESIAN_POINT('Ctrl Pts',(5.43679773227948,-1.13485587203849,-4.01483983279907));
#6723=CARTESIAN_POINT('Ctrl Pts',(5.35911766012771,-2.44050637155405,-3.1362379149185));
#6724=CARTESIAN_POINT('Ctrl Pts',(5.329368000481,-2.84678214569315,-2.71056813036084));
#6725=CARTESIAN_POINT('Ctrl Pts',(7.36726671258676,2.84740827328965,-1.50584509624218));
#6726=CARTESIAN_POINT('Ctrl Pts',(7.31932453261096,2.48452875995174,-2.19202741422533));
#6727=CARTESIAN_POINT('Ctrl Pts',(7.22345194013007,1.24417143185345,-3.28808183132752));
#6728=CARTESIAN_POINT('Ctrl Pts',(7.07963716767338,-1.24417143185342,-3.28808183132752));
#6729=CARTESIAN_POINT('Ctrl Pts',(6.98376457519251,-2.48452875995172,-2.19202741422535));
#6730=CARTESIAN_POINT('Ctrl Pts',(6.9358223952167,-2.84740827328965,-1.50584509624221));
#6731=CARTESIAN_POINT('Ctrl Pts',(7.2302560606791,3.05718837960027,-1.61678680675847));
#6732=CARTESIAN_POINT('Ctrl Pts',(7.18231388070327,2.66757406198433,-2.35352295678785));
#6733=CARTESIAN_POINT('Ctrl Pts',(7.0864412882224,1.33583458310969,-3.53032814444121));
#6734=CARTESIAN_POINT('Ctrl Pts',(6.94262651576571,-1.33583458310965,-3.53032814444122));
#6735=CARTESIAN_POINT('Ctrl Pts',(6.84675392328484,-2.6675740619843,-2.35352295678788));
#6736=CARTESIAN_POINT('Ctrl Pts',(6.79881174330904,-3.05718837960025,-1.6167868067585));
#6737=CARTESIAN_POINT('Ctrl Pts',(7.09324540877142,3.26696848591087,-1.72772851727475));
#6738=CARTESIAN_POINT('Ctrl Pts',(7.04530322879561,2.85061936401694,-2.51501849935038));
#6739=CARTESIAN_POINT('Ctrl Pts',(6.94943063631474,1.42749773436594,-3.7725744575549));
#6740=CARTESIAN_POINT('Ctrl Pts',(6.80561586385804,-1.42749773436588,-3.77257445755492));
#6741=CARTESIAN_POINT('Ctrl Pts',(6.70974327137717,-2.85061936401691,-2.51501849935041));
#6742=CARTESIAN_POINT('Ctrl Pts',(6.66180109140136,-3.26696848591084,-1.72772851727479));
#6743=CARTESIAN_POINT('Ctrl Pts',(6.95623475686376,3.47674859222147,-1.83867022779103));
#6744=CARTESIAN_POINT('Ctrl Pts',(6.90829257688794,3.03366466604953,-2.67651404191289));
#6745=CARTESIAN_POINT('Ctrl Pts',(6.81241998440707,1.51916088562219,-4.01482077066858));
#6746=CARTESIAN_POINT('Ctrl Pts',(6.66860521195038,-1.51916088562212,-4.01482077066861));
#6747=CARTESIAN_POINT('Ctrl Pts',(6.57273261946951,-3.03366466604949,-2.67651404191294));
#6748=CARTESIAN_POINT('Ctrl Pts',(6.5247904394937,-3.47674859222144,-1.83867022779109));
#6749=CARTESIAN_POINT('Ctrl Pts',(6.90165719587644,2.84677340648494,-2.71056479661449));
#6750=CARTESIAN_POINT('Ctrl Pts',(6.87190753622973,2.44048989744138,-3.13623137002149));
#6751=CARTESIAN_POINT('Ctrl Pts',(6.79422746407799,1.13481420380713,-4.01482077066858));
#6752=CARTESIAN_POINT('Ctrl Pts',(6.68679773227946,-1.13481420380722,-4.01482077066861));
#6753=CARTESIAN_POINT('Ctrl Pts',(6.60911766012771,-2.44048989744134,-3.13623137002152));
#6754=CARTESIAN_POINT('Ctrl Pts',(6.579368000481,-2.8467734064849,-2.71056479661452));
#6755=CARTESIAN_POINT('Ctrl Pts',(8.61725732794301,2.84742374204162,-1.50585106350619));
#6756=CARTESIAN_POINT('Ctrl Pts',(8.56931510768575,2.48454251156628,-2.19203770104955));
#6757=CARTESIAN_POINT('Ctrl Pts',(8.47344247492343,1.24413767428607,-3.2880837711184));
#6758=CARTESIAN_POINT('Ctrl Pts',(8.32962762190384,-1.24413767428604,-3.28808377111841));
#6759=CARTESIAN_POINT('Ctrl Pts',(8.23375498914152,-2.48454251156627,-2.19203770104957));
#6760=CARTESIAN_POINT('Ctrl Pts',(8.18581276888425,-2.84742374204161,-1.50585106350622));
#6761=CARTESIAN_POINT('Ctrl Pts',(8.48024984453137,3.05719906438292,-1.61679008096992));
#6762=CARTESIAN_POINT('Ctrl Pts',(8.43230762427411,2.66758365803813,-2.35352944129621));
#6763=CARTESIAN_POINT('Ctrl Pts',(8.33643499151179,1.33579575025379,-3.53032338680587));
#6764=CARTESIAN_POINT('Ctrl Pts',(8.1926201384922,-1.33579575025375,-3.53032338680589));
#6765=CARTESIAN_POINT('Ctrl Pts',(8.09674750572989,-2.66758365803811,-2.35352944129624));
#6766=CARTESIAN_POINT('Ctrl Pts',(8.04880528547262,-3.0571990643829,-1.61679008096995));
#6767=CARTESIAN_POINT('Ctrl Pts',(8.34324236111974,3.26697438672422,-1.72772909843364));
#6768=CARTESIAN_POINT('Ctrl Pts',(8.29530014086248,2.85062480450999,-2.51502118154286));
#6769=CARTESIAN_POINT('Ctrl Pts',(8.19942750810016,1.42745382622151,-3.77256300249335));
#6770=CARTESIAN_POINT('Ctrl Pts',(8.05561265508056,-1.42745382622146,-3.77256300249337));
#6771=CARTESIAN_POINT('Ctrl Pts',(7.95974002231824,-2.85062480450996,-2.5150211815429));
#6772=CARTESIAN_POINT('Ctrl Pts',(7.91179780206098,-3.2669743867242,-1.72772909843368));
#6773=CARTESIAN_POINT('Ctrl Pts',(8.20623487770811,3.47674970906552,-1.83866811589737));
#6774=CARTESIAN_POINT('Ctrl Pts',(8.15829265745084,3.03366595098184,-2.67651292178951));
#6775=CARTESIAN_POINT('Ctrl Pts',(8.06242002468851,1.51911190218921,-4.01480261818081));
#6776=CARTESIAN_POINT('Ctrl Pts',(7.91860517166893,-1.51911190218915,-4.01480261818084));
#6777=CARTESIAN_POINT('Ctrl Pts',(7.82273253890661,-3.0336659509818,-2.67651292178956));
#6778=CARTESIAN_POINT('Ctrl Pts',(7.77479031864935,-3.47674970906549,-1.83866811589743));
#6779=CARTESIAN_POINT('Ctrl Pts',(8.15165719587644,2.84676559888789,-2.71056162195416));
#6780=CARTESIAN_POINT('Ctrl Pts',(8.12190753622973,2.44047517949096,-3.13622513744625));
#6781=CARTESIAN_POINT('Ctrl Pts',(8.04422746407799,1.13477697746454,-4.0148026181808));
#6782=CARTESIAN_POINT('Ctrl Pts',(7.93679773227946,-1.13477697746461,-4.01480261818084));
#6783=CARTESIAN_POINT('Ctrl Pts',(7.85911766012771,-2.44047517949091,-3.13622513744629));
#6784=CARTESIAN_POINT('Ctrl Pts',(7.829368000481,-2.84676559888785,-2.71056162195421));
#6785=CARTESIAN_POINT('Ctrl Pts',(9.86724850229305,2.84743825981283,-1.50585671923049));
#6786=CARTESIAN_POINT('Ctrl Pts',(9.81930624523776,2.48455541132411,-2.19204739615685));
#6787=CARTESIAN_POINT('Ctrl Pts',(9.72343357567744,1.24410760572175,-3.28808539684982));
#6788=CARTESIAN_POINT('Ctrl Pts',(9.57961864906181,-1.24410760572175,-3.28808539684982));
#6789=CARTESIAN_POINT('Ctrl Pts',(9.48374597950147,-2.48455541132411,-2.19204739615685));
#6790=CARTESIAN_POINT('Ctrl Pts',(9.4358037224462,-2.84743825981283,-1.50585671923049));
#6791=CARTESIAN_POINT('Ctrl Pts',(9.73024399756275,3.0572090829841,-1.61679320836503));
#6792=CARTESIAN_POINT('Ctrl Pts',(9.68230174050747,2.66759264911214,-2.35353556368343));
#6793=CARTESIAN_POINT('Ctrl Pts',(9.58642907094713,1.33576103338308,-3.53031870181354));
#6794=CARTESIAN_POINT('Ctrl Pts',(9.44261414433152,-1.33576103338307,-3.53031870181354));
#6795=CARTESIAN_POINT('Ctrl Pts',(9.34674147477118,-2.66759264911214,-2.35353556368344));
#6796=CARTESIAN_POINT('Ctrl Pts',(9.29879921771591,-3.0572090829841,-1.61679320836504));
#6797=CARTESIAN_POINT('Ctrl Pts',(9.59323949283245,3.26697990615537,-1.72772969749955));
#6798=CARTESIAN_POINT('Ctrl Pts',(9.54529723577717,2.85062988690018,-2.51502373121002));
#6799=CARTESIAN_POINT('Ctrl Pts',(9.44942456621684,1.42741446104443,-3.77255200677727));
#6800=CARTESIAN_POINT('Ctrl Pts',(9.30560963960122,-1.42741446104441,-3.77255200677727));
#6801=CARTESIAN_POINT('Ctrl Pts',(9.20973697004088,-2.85062988690017,-2.51502373121004));
#6802=CARTESIAN_POINT('Ctrl Pts',(9.1617947129856,-3.26697990615537,-1.72772969749957));
#6803=CARTESIAN_POINT('Ctrl Pts',(9.45623498810215,3.47675072932665,-1.83866618663408));
#6804=CARTESIAN_POINT('Ctrl Pts',(9.40829273104687,3.03366712468821,-2.6765118987366));
#6805=CARTESIAN_POINT('Ctrl Pts',(9.31242006148653,1.51906788870579,-4.014785311741));
#6806=CARTESIAN_POINT('Ctrl Pts',(9.16860513487091,-1.51906788870575,-4.01478531174101));
#6807=CARTESIAN_POINT('Ctrl Pts',(9.07273246531058,-3.03366712468819,-2.67651189873662));
#6808=CARTESIAN_POINT('Ctrl Pts',(9.02479020825531,-3.47675072932664,-1.8386661866341));
#6809=CARTESIAN_POINT('Ctrl Pts',(9.40165719587644,2.84675858147378,-2.71055859525787));
#6810=CARTESIAN_POINT('Ctrl Pts',(9.37190753622973,2.44046195109913,-3.1362191953578));
#6811=CARTESIAN_POINT('Ctrl Pts',(9.29422746407799,1.13474351868581,-4.01478531174101));
#6812=CARTESIAN_POINT('Ctrl Pts',(9.18679773227947,-1.13474351868577,-4.01478531174101));
#6813=CARTESIAN_POINT('Ctrl Pts',(9.10911766012771,-2.4404619510991,-3.13621919535782));
#6814=CARTESIAN_POINT('Ctrl Pts',(9.079368000481,-2.84675858147374,-2.7105585952579));
#6815=CARTESIAN_POINT('Ctrl Pts',(11.102826855619,2.7325876658857,-1.7059759760899));
#6816=CARTESIAN_POINT('Ctrl Pts',(11.0564761776969,2.33512269759968,-2.34262495894918));
#6817=CARTESIAN_POINT('Ctrl Pts',(10.9637748218525,1.07966271388233,-3.32492883043245));
#6818=CARTESIAN_POINT('Ctrl Pts',(10.8247124167047,-1.31450087230183,-3.2393423413749));
#6819=CARTESIAN_POINT('Ctrl Pts',(10.7320006894791,-2.49670104301917,-2.16966721227558));
#6820=CARTESIAN_POINT('Ctrl Pts',(10.6856396401757,-2.84766280119442,-1.50605642114679));
#6821=CARTESIAN_POINT('Ctrl Pts',(10.965701366658,2.93405695958231,-1.83175484103065));
#6822=CARTESIAN_POINT('Ctrl Pts',(10.9193506887358,2.50728753844033,-2.515342929453));
#6823=CARTESIAN_POINT('Ctrl Pts',(10.8266493328915,1.15926450932041,-3.57007048550964));
#6824=CARTESIAN_POINT('Ctrl Pts',(10.6875869277437,-1.41141690746236,-3.47817384226539));
#6825=CARTESIAN_POINT('Ctrl Pts',(10.594875200518,-2.6807787953959,-2.32963328629069));
#6826=CARTESIAN_POINT('Ctrl Pts',(10.5485141512146,-3.05761639953827,-1.6170955388387));
#6827=CARTESIAN_POINT('Ctrl Pts',(10.828575877697,3.13552625327892,-1.9575337059714));
#6828=CARTESIAN_POINT('Ctrl Pts',(10.7822251997748,2.67945237928098,-2.68806089995681));
#6829=CARTESIAN_POINT('Ctrl Pts',(10.6895238439304,1.23886630475848,-3.81521214058682));
#6830=CARTESIAN_POINT('Ctrl Pts',(10.5504614387827,-1.50833294262289,-3.71700534315589));
#6831=CARTESIAN_POINT('Ctrl Pts',(10.4577497115571,-2.86485654777264,-2.48959936030581));
#6832=CARTESIAN_POINT('Ctrl Pts',(10.4113886622536,-3.26756999788213,-1.72813465653059));
#6833=CARTESIAN_POINT('Ctrl Pts',(10.6914503887359,3.33699554697554,-2.08331257091215));
#6834=CARTESIAN_POINT('Ctrl Pts',(10.6450997108137,2.85161722012163,-2.86077887046062));
#6835=CARTESIAN_POINT('Ctrl Pts',(10.5523983549694,1.31846810019657,-4.060353795664));
#6836=CARTESIAN_POINT('Ctrl Pts',(10.4133359498216,-1.60524897778342,-3.95583684404638));
#6837=CARTESIAN_POINT('Ctrl Pts',(10.320624222596,-3.04893430014939,-2.64956543432092));
#6838=CARTESIAN_POINT('Ctrl Pts',(10.2742631732926,-3.47752359622599,-1.83917377422248));
#6839=CARTESIAN_POINT('Ctrl Pts',(10.6511271608452,2.84811859529839,-2.71144775012001));
#6840=CARTESIAN_POINT('Ctrl Pts',(10.6426113435813,2.73171713488881,-2.83319832190457));
#6841=CARTESIAN_POINT('Ctrl Pts',(10.6340983716353,2.60759935714515,-2.94754525934051));
#6842=CARTESIAN_POINT('Ctrl Pts',(10.625585572441,2.47683252453344,-3.05366724755375));
#6843=CARTESIAN_POINT('Ctrl Pts',(10.6218467434829,2.41939961564344,-3.10027611892081));
#6844=CARTESIAN_POINT('Ctrl Pts',(10.6181079136966,2.36068334109682,-3.14529863695637));
#6845=CARTESIAN_POINT('Ctrl Pts',(10.6143687919012,2.30077187014575,-3.1886646310268));
#6846=CARTESIAN_POINT('Ctrl Pts',(10.6089168023024,2.21341533715529,-3.25189630989463));
#6847=CARTESIAN_POINT('Ctrl Pts',(10.6034641426978,2.12351330806985,-3.31160904245313));
#6848=CARTESIAN_POINT('Ctrl Pts',(10.5981005515451,2.03127319304859,-3.36743710409997));
#6849=CARTESIAN_POINT('Ctrl Pts',(10.5974339725144,2.01980973046982,-3.37437533152289));
#6850=CARTESIAN_POINT('Ctrl Pts',(10.5967687691587,2.00831021126505,-3.38125352367139));
#6851=CARTESIAN_POINT('Ctrl Pts',(10.596105113731,1.9967750816594,-3.38807094926279));
#6852=CARTESIAN_POINT('Ctrl Pts',(10.5901000063047,1.89239909139864,-3.449758643416));
#6853=CARTESIAN_POINT('Ctrl Pts',(10.5841550208651,1.78516834568221,-3.50656836848592));
#6854=CARTESIAN_POINT('Ctrl Pts',(10.5781918261005,1.67557705661834,-3.55828266075338));
#6855=CARTESIAN_POINT('Ctrl Pts',(10.5722246358433,1.56591233859679,-3.6100316029151));
#6856=CARTESIAN_POINT('Ctrl Pts',(10.5662388498881,1.4538822869375,-3.65667878953976));
#6857=CARTESIAN_POINT('Ctrl Pts',(10.5601720413959,1.33997712745255,-3.69799569478362));
#6858=CARTESIAN_POINT('Ctrl Pts',(10.5579472993162,1.29820729052431,-3.71314689954221));
#6859=CARTESIAN_POINT('Ctrl Pts',(10.5557115288928,1.25618558336911,-3.72758169383098));
#6860=CARTESIAN_POINT('Ctrl Pts',(10.553461263821,1.21393717344435,-3.74129018761173));
#6861=CARTESIAN_POINT('Ctrl Pts',(10.5534608102716,1.21392865811811,-3.74129295061032));
#6862=CARTESIAN_POINT('Ctrl Pts',(10.5534603567216,1.21392014278266,-3.7412957135794));
#6863=CARTESIAN_POINT('Ctrl Pts',(10.553459903171,1.21391162743801,-3.74129847651897));
#6864=CARTESIAN_POINT('Ctrl Pts',(10.5474425313702,1.10093636793918,-3.77795510385333));
#6865=CARTESIAN_POINT('Ctrl Pts',(10.5413175017578,0.986208288849423,-3.80945458848442));
#6866=CARTESIAN_POINT('Ctrl Pts',(10.5351573209224,0.870232321763314,-3.83568283978526));
#6867=CARTESIAN_POINT('Ctrl Pts',(10.5290007304002,0.75432394847934,-3.86189580458086));
#6868=CARTESIAN_POINT('Ctrl Pts',(10.5228093348457,0.637169173319156,-3.88284400980358));
#6869=CARTESIAN_POINT('Ctrl Pts',(10.5166366967313,0.519271500073078,-3.898455756584));
#6870=CARTESIAN_POINT('Ctrl Pts',(10.5104664725844,0.401419933716071,-3.91406139799307));
#6871=CARTESIAN_POINT('Ctrl Pts',(10.5043151500659,0.282822465141323,-3.92433507136264));
#6872=CARTESIAN_POINT('Ctrl Pts',(10.4982820270001,0.163987241636089,-3.92912540483231));
#6873=CARTESIAN_POINT('Ctrl Pts',(10.4922501071092,0.0451757172244269,-3.93391478297444));
#6874=CARTESIAN_POINT('Ctrl Pts',(10.486242686869,-0.0738614654372977,-3.93338541360083));
#6875=CARTESIAN_POINT('Ctrl Pts',(10.4802349464414,-0.192642255022724,-3.92759735592231));
#6876=CARTESIAN_POINT('Ctrl Pts',(10.4742254144236,-0.311458466663116,-3.92180757216588));
#6877=CARTESIAN_POINT('Ctrl Pts',(10.4682155029908,-0.430024800662094,-3.91075526859723));
#6878=CARTESIAN_POINT('Ctrl Pts',(10.4622839172821,-0.547828062706187,-3.89431655465985));
#6879=CARTESIAN_POINT('Ctrl Pts',(10.4563515943019,-0.665645967208858,-3.87787579745826));
#6880=CARTESIAN_POINT('Ctrl Pts',(10.4504973814454,-0.782693714943688,-3.85604789527817));
#6881=CARTESIAN_POINT('Ctrl Pts',(10.4446463021523,-0.89847165460343,-3.82897684250146));
#6882=CARTESIAN_POINT('Ctrl Pts',(10.4387907650912,-1.01433780212464,-3.80188516507311));
#6883=CARTESIAN_POINT('Ctrl Pts',(10.4329380781062,-1.12893399373693,-3.76954177223671));
#6884=CARTESIAN_POINT('Ctrl Pts',(10.4270312817244,-1.24175748432463,-3.73207010560792));
#6885=CARTESIAN_POINT('Ctrl Pts',(10.4228594183156,-1.3214426743339,-3.70560454546858));
#6886=CARTESIAN_POINT('Ctrl Pts',(10.4186601428766,-1.40024358005016,-3.67658170501823));
#6887=CARTESIAN_POINT('Ctrl Pts',(10.4144092301524,-1.47798418218269,-3.64505946246045));
#6888=CARTESIAN_POINT('Ctrl Pts',(10.4144087763743,-1.47799248086676,-3.64505609751183));
#6889=CARTESIAN_POINT('Ctrl Pts',(10.4144083225956,-1.47800077953875,-3.64505273253473));
#6890=CARTESIAN_POINT('Ctrl Pts',(10.4144078688164,-1.47800907819868,-3.64504936752915));
#6891=CARTESIAN_POINT('Ctrl Pts',(10.4081994866578,-1.59154721528751,-3.59901103502734));
#6892=CARTESIAN_POINT('Ctrl Pts',(10.4018766600276,-1.70294647533206,-3.5475869456103));
#6893=CARTESIAN_POINT('Ctrl Pts',(10.3955144750265,-1.81172128060229,-3.49103629418496));
#6894=CARTESIAN_POINT('Ctrl Pts',(10.3891567721835,-1.92041945404185,-3.43452548268334));
#6895=CARTESIAN_POINT('Ctrl Pts',(10.3827601083259,-2.02649714329538,-3.37289561599235));
#6896=CARTESIAN_POINT('Ctrl Pts',(10.3763800404594,-2.12949887542201,-3.30643628014277));
#6897=CARTESIAN_POINT('Ctrl Pts',(10.3700031717913,-2.23244895873014,-3.24001026942378));
#6898=CARTESIAN_POINT('Ctrl Pts',(10.3637052866195,-2.33226726847003,-3.16866913269694));
#6899=CARTESIAN_POINT('Ctrl Pts',(10.357507269449,-2.42851430469666,-3.09276322709174));
#6900=CARTESIAN_POINT('Ctrl Pts',(10.3485264698033,-2.56797428440723,-2.98277712808411));
#6901=CARTESIAN_POINT('Ctrl Pts',(10.3395467174008,-2.70016255934201,-2.86349404392066));
#6902=CARTESIAN_POINT('Ctrl Pts',(10.3305630683185,-2.82393045013914,-2.73594564924192));
#6903=CARTESIAN_POINT('Ctrl Pts',(10.3299882949333,-2.83184911313627,-2.72778510980977));
#6904=CARTESIAN_POINT('Ctrl Pts',(10.3294135057467,-2.83973329278916,-2.71959072700772));
#6905=CARTESIAN_POINT('Ctrl Pts',(10.3288386995335,-2.84758268181463,-2.71136276737431));
#6906=CARTESIAN_POINT('Origin',(11.0238490761436,0.781229937496414,-0.42649944676949));
#6907=CARTESIAN_POINT('Ctrl Pts',(4.24229308138461,-2.84736462220321,1.50582860737967));
#6908=CARTESIAN_POINT('Ctrl Pts',(4.19435102145226,-2.48448991370969,2.19199864350045));
#6909=CARTESIAN_POINT('Ctrl Pts',(4.09847854901485,-1.24427690485953,3.28807512492806));
#6910=CARTESIAN_POINT('Ctrl Pts',(3.95466401664509,1.24427690485951,3.28807512492806));
#6911=CARTESIAN_POINT('Ctrl Pts',(3.85879154420768,2.48448991370968,2.19199864350047));
#6912=CARTESIAN_POINT('Ctrl Pts',(3.81084948427533,2.84736462220321,1.50582860737969));
#6913=CARTESIAN_POINT('Ctrl Pts',(4.10527351983419,-3.05715816943107,1.61677791207915));
#6914=CARTESIAN_POINT('Ctrl Pts',(4.05733145990184,-2.66754688786205,2.35350488943491));
#6915=CARTESIAN_POINT('Ctrl Pts',(3.96145898746443,-1.33595510566621,3.53034017894723));
#6916=CARTESIAN_POINT('Ctrl Pts',(3.81764445509467,1.33595510566618,3.53034017894724));
#6917=CARTESIAN_POINT('Ctrl Pts',(3.72177198265727,2.66754688786203,2.35350488943492));
#6918=CARTESIAN_POINT('Ctrl Pts',(3.67382992272492,3.05715816943106,1.61677791207918));
#6919=CARTESIAN_POINT('Ctrl Pts',(3.96825395828378,-3.26695171665892,1.72772721677864));
#6920=CARTESIAN_POINT('Ctrl Pts',(3.92031189835143,-2.8506038620144,2.51501113536934));
#6921=CARTESIAN_POINT('Ctrl Pts',(3.82443942591402,-1.42763330647289,3.77260523296638));
#6922=CARTESIAN_POINT('Ctrl Pts',(3.68062489354426,1.42763330647285,3.77260523296639));
#6923=CARTESIAN_POINT('Ctrl Pts',(3.58475242110685,2.85060386201438,2.51501113536938));
#6924=CARTESIAN_POINT('Ctrl Pts',(3.5368103611745,3.2669517166589,1.72772721677867));
#6925=CARTESIAN_POINT('Ctrl Pts',(3.83123439673337,-3.47674526388677,1.83867652147811));
#6926=CARTESIAN_POINT('Ctrl Pts',(3.78329233680102,-3.03366083616676,2.67651738130379));
#6927=CARTESIAN_POINT('Ctrl Pts',(3.68741986436361,-1.51931150727957,4.01487028698555));
#6928=CARTESIAN_POINT('Ctrl Pts',(3.54360533199384,1.51931150727952,4.01487028698557));
#6929=CARTESIAN_POINT('Ctrl Pts',(3.44773285955643,3.03366083616673,2.67651738130383));
#6930=CARTESIAN_POINT('Ctrl Pts',(3.39979079962409,3.47674526388675,1.83867652147816));
#6931=CARTESIAN_POINT('Ctrl Pts',(3.77665719587644,-2.84679740187303,2.71057345644603));
#6932=CARTESIAN_POINT('Ctrl Pts',(3.74690753622973,-2.44053513068406,3.13624837122676));
#6933=CARTESIAN_POINT('Ctrl Pts',(3.66922746407795,-1.1349286129563,4.01487028698564));
#6934=CARTESIAN_POINT('Ctrl Pts',(3.56179773227949,1.13492861295628,4.01487028698554));
#6935=CARTESIAN_POINT('Ctrl Pts',(3.48411766012771,2.44053513068398,3.13624837122682));
#6936=CARTESIAN_POINT('Ctrl Pts',(3.454368000481,2.84679740187295,2.71057345644611));
#6937=CARTESIAN_POINT('Ctrl Pts',(5.492281984131,-2.84738302772049,1.50583549468422));
#6938=CARTESIAN_POINT('Ctrl Pts',(5.44433987239449,-2.48450630084475,2.19201072670901));
#6939=CARTESIAN_POINT('Ctrl Pts',(5.34846734815293,-1.24423052896037,3.28807818231816));
#6940=CARTESIAN_POINT('Ctrl Pts',(5.20465271217485,1.24423052896033,3.28807818231818));
#6941=CARTESIAN_POINT('Ctrl Pts',(5.10878018793329,2.48450630084472,2.19201072670904));
#6942=CARTESIAN_POINT('Ctrl Pts',(5.06083807619678,2.84738302772047,1.50583549468426));
#6943=CARTESIAN_POINT('Ctrl Pts',(5.35526617346927,-3.05717091855179,1.61678159827943));
#6944=CARTESIAN_POINT('Ctrl Pts',(5.30732406173276,-2.66755836357639,2.35351246446573));
#6945=CARTESIAN_POINT('Ctrl Pts',(5.2114515374912,-1.33590224851384,3.53033536375158));
#6946=CARTESIAN_POINT('Ctrl Pts',(5.06763690151313,1.33590224851378,3.53033536375161));
#6947=CARTESIAN_POINT('Ctrl Pts',(4.97176437727157,2.66755836357635,2.35351246446577));
#6948=CARTESIAN_POINT('Ctrl Pts',(4.92382226553506,3.05717091855177,1.61678159827947));
#6949=CARTESIAN_POINT('Ctrl Pts',(5.21825036280756,-3.26695880938309,1.72772770187462));
#6950=CARTESIAN_POINT('Ctrl Pts',(5.17030825107105,-2.85061042630803,2.51501420222245));
#6951=CARTESIAN_POINT('Ctrl Pts',(5.07443572682949,-1.42757396806733,3.772592545185));
#6952=CARTESIAN_POINT('Ctrl Pts',(4.93062109085141,1.42757396806726,3.77259254518503));
#6953=CARTESIAN_POINT('Ctrl Pts',(4.83474856660984,2.85061042630798,2.5150142022225));
#6954=CARTESIAN_POINT('Ctrl Pts',(4.78680645487334,3.26695880938306,1.72772770187468));
#6955=CARTESIAN_POINT('Ctrl Pts',(5.08123455214584,-3.4767467002144,1.83867380546982));
#6956=CARTESIAN_POINT('Ctrl Pts',(5.03329244040933,-3.03366248903967,2.67651593997917));
#6957=CARTESIAN_POINT('Ctrl Pts',(4.93741991616776,-1.51924568762079,4.01484972661843));
#6958=CARTESIAN_POINT('Ctrl Pts',(4.79360528018969,1.51924568762071,4.01484972661846));
#6959=CARTESIAN_POINT('Ctrl Pts',(4.69773275594812,3.03366248903961,2.67651593997923));
#6960=CARTESIAN_POINT('Ctrl Pts',(4.64979064421162,3.47674670021436,1.83867380546989));
#6961=CARTESIAN_POINT('Ctrl Pts',(5.02665719587644,-2.84678691836037,2.71056986067545));
#6962=CARTESIAN_POINT('Ctrl Pts',(4.99690753622973,-2.44051536841681,3.13624131191695));
#6963=CARTESIAN_POINT('Ctrl Pts',(4.919227464078,-1.1348786279445,4.01484972661831));
#6964=CARTESIAN_POINT('Ctrl Pts',(4.81179773227947,1.13487862794425,4.0148497266185));
#6965=CARTESIAN_POINT('Ctrl Pts',(4.73411766012771,2.44051536841673,3.13624131191701));
#6966=CARTESIAN_POINT('Ctrl Pts',(4.704368000481,2.8467869183603,2.71056986067553));
#6967=CARTESIAN_POINT('Ctrl Pts',(6.74227163450666,-2.84740014697697,1.50584198663232));
#6968=CARTESIAN_POINT('Ctrl Pts',(6.69432947615129,-2.48452153278042,2.19202202872339));
#6969=CARTESIAN_POINT('Ctrl Pts',(6.59845690529086,-1.24418990160601,3.28808072348868));
#6970=CARTESIAN_POINT('Ctrl Pts',(6.45464217607506,1.24418990160599,3.28808072348869));
#6971=CARTESIAN_POINT('Ctrl Pts',(6.35876960521463,2.4845215327804,2.1920220287234));
#6972=CARTESIAN_POINT('Ctrl Pts',(6.31082744685926,2.84740014697696,1.50584198663235));
#6973=CARTESIAN_POINT('Ctrl Pts',(6.60525932033858,-3.05718276224204,1.61678511152717));
#6974=CARTESIAN_POINT('Ctrl Pts',(6.55731716198321,-2.66756901396511,2.35351956688725));
#6975=CARTESIAN_POINT('Ctrl Pts',(6.46144459112278,-1.33585577151278,3.53033054359509));
#6976=CARTESIAN_POINT('Ctrl Pts',(6.31762986190698,1.33585577151274,3.53033054359509));
#6977=CARTESIAN_POINT('Ctrl Pts',(6.22175729104655,2.66756901396509,2.35351956688727));
#6978=CARTESIAN_POINT('Ctrl Pts',(6.17381513269119,3.05718276224202,1.61678511152721));
#6979=CARTESIAN_POINT('Ctrl Pts',(6.4682470061705,-3.26696537750712,1.72772823642201));
#6980=CARTESIAN_POINT('Ctrl Pts',(6.42030484781513,-2.85061649514982,2.51501710505113));
#6981=CARTESIAN_POINT('Ctrl Pts',(6.3244322769547,-1.42752164141955,3.77258036370151));
#6982=CARTESIAN_POINT('Ctrl Pts',(6.1806175477389,1.42752164141951,3.77258036370152));
#6983=CARTESIAN_POINT('Ctrl Pts',(6.08474497687847,2.85061649514979,2.51501710505116));
#6984=CARTESIAN_POINT('Ctrl Pts',(6.0368028185231,3.2669653775071,1.72772823642205));
#6985=CARTESIAN_POINT('Ctrl Pts',(6.33123469200243,-3.4767479927722,1.83867136131686));
#6986=CARTESIAN_POINT('Ctrl Pts',(6.28329253364706,-3.03366397633451,2.676514643215));
#6987=CARTESIAN_POINT('Ctrl Pts',(6.18741996278662,-1.51918751132632,4.01483018380791));
#6988=CARTESIAN_POINT('Ctrl Pts',(6.04360523357082,1.51918751132626,4.01483018380792));
#6989=CARTESIAN_POINT('Ctrl Pts',(5.94773266271039,3.03366397633447,2.67651464321504));
#6990=CARTESIAN_POINT('Ctrl Pts',(5.89979050435502,3.47674799277217,1.83867136131692));
#6991=CARTESIAN_POINT('Ctrl Pts',(6.27665719587644,-2.84677764951821,2.71056644286375));
#6992=CARTESIAN_POINT('Ctrl Pts',(6.24690753622973,-2.44049789590145,3.13623460198065));
#6993=CARTESIAN_POINT('Ctrl Pts',(6.16922746407796,-1.13483443443749,4.01483018380789));
#6994=CARTESIAN_POINT('Ctrl Pts',(6.06179773227948,1.13483443443743,4.01483018380793));
#6995=CARTESIAN_POINT('Ctrl Pts',(5.98411766012771,2.44049789590139,3.13623460198069));
#6996=CARTESIAN_POINT('Ctrl Pts',(5.954368000481,2.84677764951816,2.71056644286381));
#6997=CARTESIAN_POINT('Ctrl Pts',(7.99226194656689,-2.84741613328985,1.50584812058205));
#6998=CARTESIAN_POINT('Ctrl Pts',(7.94431974598207,-2.48453574834069,2.19203263547465));
#6999=CARTESIAN_POINT('Ctrl Pts',(7.84844713289218,-1.24415405273242,3.28808284427961));
#7000=CARTESIAN_POINT('Ctrl Pts',(7.70463231921746,1.24415405273241,3.28808284427962));
#7001=CARTESIAN_POINT('Ctrl Pts',(7.60875970612758,2.48453574834068,2.19203263547466));
#7002=CARTESIAN_POINT('Ctrl Pts',(7.56081750554275,2.84741613328985,1.50584812058207));
#7003=CARTESIAN_POINT('Ctrl Pts',(7.85525290394152,-3.05719381006904,1.61678846281894));
#7004=CARTESIAN_POINT('Ctrl Pts',(7.8073107033567,-2.66757894004992,2.35352624658332));
#7005=CARTESIAN_POINT('Ctrl Pts',(7.71143809026681,-1.33581460901229,3.53032575779908));
#7006=CARTESIAN_POINT('Ctrl Pts',(7.5676232765921,1.33581460901226,3.5303257577991));
#7007=CARTESIAN_POINT('Ctrl Pts',(7.47175066350222,2.66757894004991,2.35352624658334));
#7008=CARTESIAN_POINT('Ctrl Pts',(7.42380846291739,3.05719381006903,1.61678846281896));
#7009=CARTESIAN_POINT('Ctrl Pts',(7.71824386131615,-3.26697148684823,1.72772880505582));
#7010=CARTESIAN_POINT('Ctrl Pts',(7.67030166073133,-2.85062213175916,2.51501985769196));
#7011=CARTESIAN_POINT('Ctrl Pts',(7.57442904764143,-1.42747516529217,3.77256867131854));
#7012=CARTESIAN_POINT('Ctrl Pts',(7.43061423396673,1.42747516529213,3.77256867131855));
#7013=CARTESIAN_POINT('Ctrl Pts',(7.33474162087684,2.85062213175914,2.51501985769199));
#7014=CARTESIAN_POINT('Ctrl Pts',(7.28679942029201,3.26697148684821,1.72772880505585));
#7015=CARTESIAN_POINT('Ctrl Pts',(7.58123481869079,-3.47674916362741,1.83866914729269));
#7016=CARTESIAN_POINT('Ctrl Pts',(7.53329261810597,-3.0336653234684,2.67651346880062));
#7017=CARTESIAN_POINT('Ctrl Pts',(7.43742000501609,-1.51913572157204,4.01481158483801));
#7018=CARTESIAN_POINT('Ctrl Pts',(7.29360519134137,1.51913572157199,4.01481158483803));
#7019=CARTESIAN_POINT('Ctrl Pts',(7.19773257825148,3.03366532346837,2.67651346880066));
#7020=CARTESIAN_POINT('Ctrl Pts',(7.14979037766666,3.47674916362739,1.83866914729274));
#7021=CARTESIAN_POINT('Ctrl Pts',(7.52665719587644,-2.84676939580033,2.71056319011889));
#7022=CARTESIAN_POINT('Ctrl Pts',(7.49690753622974,-2.44048233697729,3.13622821610778));
#7023=CARTESIAN_POINT('Ctrl Pts',(7.41922746407797,-1.13479508100687,4.01481158483798));
#7024=CARTESIAN_POINT('Ctrl Pts',(7.31179773227947,1.13479508100694,4.01481158483804));
#7025=CARTESIAN_POINT('Ctrl Pts',(7.23411766012771,2.44048233697723,3.13622821610782));
#7026=CARTESIAN_POINT('Ctrl Pts',(7.204368000481,2.84676939580028,2.71056319011894));
#7027=CARTESIAN_POINT('Ctrl Pts',(9.24225284891195,-2.84743111333128,1.50585392860498));
#7028=CARTESIAN_POINT('Ctrl Pts',(9.19431060985147,-2.48454906208509,2.19204261884696));
#7029=CARTESIAN_POINT('Ctrl Pts',(9.09843795828593,-1.24412221602484,3.2880846196523));
#7030=CARTESIAN_POINT('Ctrl Pts',(8.9546230676599,1.24412221602484,3.2880846196523));
#7031=CARTESIAN_POINT('Ctrl Pts',(8.85875041609436,2.48454906208509,2.19204261884696));
#7032=CARTESIAN_POINT('Ctrl Pts',(8.81080817703388,2.84743111333128,1.50585392860498));
#7033=CARTESIAN_POINT('Ctrl Pts',(9.10524687731388,-3.05720415235532,1.61679166242786));
#7034=CARTESIAN_POINT('Ctrl Pts',(9.0573046382534,-2.66758822497045,2.35353254556472));
#7035=CARTESIAN_POINT('Ctrl Pts',(8.96143198668786,-1.33577791822989,3.53032103408329));
#7036=CARTESIAN_POINT('Ctrl Pts',(8.81761709606184,1.33577791822988,3.53032103408329));
#7037=CARTESIAN_POINT('Ctrl Pts',(8.7217444444963,2.66758822497045,2.35353254556473));
#7038=CARTESIAN_POINT('Ctrl Pts',(8.67380220543582,3.05720415235531,1.61679166242787));
#7039=CARTESIAN_POINT('Ctrl Pts',(8.96824090571582,-3.26697719137936,1.72772939625073));
#7040=CARTESIAN_POINT('Ctrl Pts',(8.92029866665534,-2.85062738785583,2.51502247228247));
#7041=CARTESIAN_POINT('Ctrl Pts',(8.82442601508979,-1.42743362043492,3.77255744851429));
#7042=CARTESIAN_POINT('Ctrl Pts',(8.68061112446378,1.4274336204349,3.77255744851431));
#7043=CARTESIAN_POINT('Ctrl Pts',(8.58473847289823,2.85062738785582,2.51502247228249));
#7044=CARTESIAN_POINT('Ctrl Pts',(8.53679623383775,3.26697719137935,1.72772939625075));
#7045=CARTESIAN_POINT('Ctrl Pts',(8.83123493411776,-3.47675023040339,1.83866713007362));
#7046=CARTESIAN_POINT('Ctrl Pts',(8.78329269505728,-3.03366655074119,2.67651239900022));
#7047=CARTESIAN_POINT('Ctrl Pts',(8.68742004349173,-1.51908932263997,4.01479386294529));
#7048=CARTESIAN_POINT('Ctrl Pts',(8.54360515286572,1.51908932263994,4.0147938629453));
#7049=CARTESIAN_POINT('Ctrl Pts',(8.44773250130017,3.03366655074117,2.67651239900024));
#7050=CARTESIAN_POINT('Ctrl Pts',(8.39979026223969,3.47675023040338,1.83866713007365));
#7051=CARTESIAN_POINT('Ctrl Pts',(8.77665719587644,-2.84676199909996,2.71056009076467));
#7052=CARTESIAN_POINT('Ctrl Pts',(8.74690753622973,-2.44046839360025,3.13622213137543));
#7053=CARTESIAN_POINT('Ctrl Pts',(8.66922746407795,-1.13475981380474,4.01479386294536));
#7054=CARTESIAN_POINT('Ctrl Pts',(8.56179773227949,1.13475981380472,4.01479386294528));
#7055=CARTESIAN_POINT('Ctrl Pts',(8.48411766012771,2.4404683936002,3.13622213137546));
#7056=CARTESIAN_POINT('Ctrl Pts',(8.454368000481,2.84676199909991,2.71056009076472));
#7057=CARTESIAN_POINT('Ctrl Pts',(10.4922442814608,-2.84744519313275,1.50585943851893));
#7058=CARTESIAN_POINT('Ctrl Pts',(10.4443020071642,-2.48456156979463,2.19205203972627));
#7059=CARTESIAN_POINT('Ctrl Pts',(10.3484293203624,-1.24409377838615,3.28808610894595));
#7060=CARTESIAN_POINT('Ctrl Pts',(10.2046143592641,1.24409377838615,3.28808610894595));
#7061=CARTESIAN_POINT('Ctrl Pts',(10.1087416724623,2.48456156979462,2.19205203972627));
#7062=CARTESIAN_POINT('Ctrl Pts',(10.0607993981656,2.84744519313275,1.50585943851893));
#7063=CARTESIAN_POINT('Ctrl Pts',(10.3552412009161,-3.05721386454218,1.61679471991055));
#7064=CARTESIAN_POINT('Ctrl Pts',(10.3072989266194,-2.66759693805657,2.3535384996387));
#7065=CARTESIAN_POINT('Ctrl Pts',(10.2114262398176,-1.33574502408184,3.5303163918033));
#7066=CARTESIAN_POINT('Ctrl Pts',(10.0676112787192,1.33574502408182,3.53031639180331));
#7067=CARTESIAN_POINT('Ctrl Pts',(9.97173859191745,2.66759693805656,2.35353849963872));
#7068=CARTESIAN_POINT('Ctrl Pts',(9.92379631762076,3.05721386454217,1.61679471991057));
#7069=CARTESIAN_POINT('Ctrl Pts',(10.2182381203711,-3.26698253595159,1.7277300013022));
#7070=CARTESIAN_POINT('Ctrl Pts',(10.1702958460745,-2.8506323063185,2.51502495955112));
#7071=CARTESIAN_POINT('Ctrl Pts',(10.0744231592728,-1.42739626977752,3.77254667466065));
#7072=CARTESIAN_POINT('Ctrl Pts',(9.93060819817435,1.42739626977749,3.77254667466066));
#7073=CARTESIAN_POINT('Ctrl Pts',(9.83473551137261,2.85063230631848,2.51502495955114));
#7074=CARTESIAN_POINT('Ctrl Pts',(9.78679323707594,3.26698253595158,1.72773000130222));
#7075=CARTESIAN_POINT('Ctrl Pts',(10.0812350398263,-3.47675120736102,1.83866528269383));
#7076=CARTESIAN_POINT('Ctrl Pts',(10.0332927655296,-3.03366767458044,2.67651141946355));
#7077=CARTESIAN_POINT('Ctrl Pts',(9.93742007872794,-1.5190475154732,4.014776957518));
#7078=CARTESIAN_POINT('Ctrl Pts',(9.79360511762951,1.51904751547316,4.01477695751801));
#7079=CARTESIAN_POINT('Ctrl Pts',(9.69773243082778,3.03366767458041,2.67651141946358));
#7080=CARTESIAN_POINT('Ctrl Pts',(9.6497901565311,3.476751207361,1.83866528269385));
#7081=CARTESIAN_POINT('Ctrl Pts',(10.0266571958764,-2.84675533252353,2.71055713420083));
#7082=CARTESIAN_POINT('Ctrl Pts',(9.99690753622973,-2.44045582656577,3.13621632697281));
#7083=CARTESIAN_POINT('Ctrl Pts',(9.91922746407798,-1.13472802780763,4.01477695751801));
#7084=CARTESIAN_POINT('Ctrl Pts',(9.81179773227947,1.13472802780759,4.01477695751801));
#7085=CARTESIAN_POINT('Ctrl Pts',(9.73411766012771,2.44045582656573,3.13621632697284));
#7086=CARTESIAN_POINT('Ctrl Pts',(9.704368000481,2.84675533252349,2.71055713420087));
#7087=CARTESIAN_POINT('Origin',(3.02384907614375,0.,0.));
#7088=CARTESIAN_POINT('Ctrl Pts',(3.02384907614375,-0.0271982295007612,
3.22179557349031));
#7089=CARTESIAN_POINT('Ctrl Pts',(3.02384907614375,0.0787467680287735,3.23416676714299));
#7090=CARTESIAN_POINT('Ctrl Pts',(3.02384907614375,0.185048789657521,3.24132583932574));
#7091=CARTESIAN_POINT('Ctrl Pts',(3.02384907614375,0.291285361330346,3.24329345860347));
#7092=CARTESIAN_POINT('Ctrl Pts',(3.02384907614375,0.398696099786925,3.24528282475387));
#7093=CARTESIAN_POINT('Ctrl Pts',(3.02384907614375,0.506040779421253,3.24196569447197));
#7094=CARTESIAN_POINT('Ctrl Pts',(3.02384907614375,0.612908356448757,3.2333169334513));
#7095=CARTESIAN_POINT('Ctrl Pts',(3.02384907614375,0.69342764175655,3.22680053179279));
#7096=CARTESIAN_POINT('Ctrl Pts',(3.02384907614375,0.773676703283155,3.21725651226085));
#7097=CARTESIAN_POINT('Ctrl Pts',(3.02384907614375,0.853484633313019,3.204655194923));
#7098=CARTESIAN_POINT('Ctrl Pts',(3.02384907614375,0.948602940134056,3.18963643715743));
#7099=CARTESIAN_POINT('Ctrl Pts',(3.02384907614375,1.04309503128853,3.17027579824669));
#7100=CARTESIAN_POINT('Ctrl Pts',(3.02384907614375,1.13674268826726,3.14672432130043));
#7101=CARTESIAN_POINT('Ctrl Pts',(3.02384907614375,1.15921157599614,3.14107361408119));
#7102=CARTESIAN_POINT('Ctrl Pts',(3.02384907614375,1.18163183734146,3.13518149603407));
#7103=CARTESIAN_POINT('Ctrl Pts',(3.02384907614375,1.20400041713337,3.12904975582882));
#7104=CARTESIAN_POINT('Ctrl Pts',(3.02384907614375,1.22668855383874,3.12283041775225));
#7105=CARTESIAN_POINT('Ctrl Pts',(3.02384907614375,1.2493272800887,3.11636326663925));
#7106=CARTESIAN_POINT('Ctrl Pts',(3.02384907614375,1.27187893963435,3.10966082396874));
#7107=CARTESIAN_POINT('Ctrl Pts',(3.02384907614375,1.37566821123953,3.07881424075653));
#7108=CARTESIAN_POINT('Ctrl Pts',(3.02384907614376,1.4777658367785,3.04294833555469));
#7109=CARTESIAN_POINT('Ctrl Pts',(3.02384907614375,1.57787399170956,3.00235617548192));
#7110=CARTESIAN_POINT('Ctrl Pts',(3.02384907614375,1.67945971177358,2.96116488779126));
#7111=CARTESIAN_POINT('Ctrl Pts',(3.02384907614375,1.77899754429907,2.91510663434206));
#7112=CARTESIAN_POINT('Ctrl Pts',(3.02384907614375,1.87617830774079,2.86443319678252));
#7113=CARTESIAN_POINT('Ctrl Pts',(3.02384907614376,1.97420990059414,2.81331610710976));
#7114=CARTESIAN_POINT('Ctrl Pts',(3.02384907614375,2.06984379056666,2.75750242593435));
#7115=CARTESIAN_POINT('Ctrl Pts',(3.02384907614375,2.1627527754763,2.69719875952457));
#7116=CARTESIAN_POINT('Ctrl Pts',(3.02384907614375,2.22372524808531,2.65762386101535));
#7117=CARTESIAN_POINT('Ctrl Pts',(3.02384907614376,2.28352394250253,2.61611417188707));
#7118=CARTESIAN_POINT('Ctrl Pts',(3.02384907614376,2.3420514723285,2.57271690759621));
#7119=CARTESIAN_POINT('Ctrl Pts',(3.02384907614376,2.36251670760645,2.55754225001589));
#7120=CARTESIAN_POINT('Ctrl Pts',(3.02384907614375,2.38282647584896,2.54213672662517));
#7121=CARTESIAN_POINT('Ctrl Pts',(3.02384907614375,2.40297645819471,2.52650211691943));
#7122=CARTESIAN_POINT('Ctrl Pts',(3.02384907614375,2.41529317891841,2.51694542758514));
#7123=CARTESIAN_POINT('Ctrl Pts',(3.02384907614376,2.42754254591775,2.50730907271123));
#7124=CARTESIAN_POINT('Ctrl Pts',(3.02384907614376,2.43972290434691,2.49759447327989));
#7125=CARTESIAN_POINT('Ctrl Pts',(3.02384907614376,2.52887669074654,2.42648873959427));
#7126=CARTESIAN_POINT('Ctrl Pts',(3.02384907614376,2.61435347490571,2.35118026521884));
#7127=CARTESIAN_POINT('Ctrl Pts',(3.02384907614375,2.69583042051309,2.27193767966696));
#7128=CARTESIAN_POINT('Ctrl Pts',(3.02384907614375,2.74846100352769,2.22075039661297));
#7129=CARTESIAN_POINT('Ctrl Pts',(3.02384907614375,2.7994224920531,2.16792047499698));
#7130=CARTESIAN_POINT('Ctrl Pts',(3.02384907614375,2.84862442584919,2.11350930842726));
#7131=CARTESIAN_POINT('Origin',(3.02384907614375,0.,0.));
#7132=CARTESIAN_POINT('Origin',(11.0238490761438,0.,0.));
#7133=CARTESIAN_POINT('Origin',(11.0238490761438,0.,0.));
#7134=CARTESIAN_POINT('',(11.0238490761438,-1.74837398213582,3.52379982655521));
#7135=CARTESIAN_POINT('Ctrl Pts',(10.7710409564111,2.84675014301221,2.71055471688623));
#7136=CARTESIAN_POINT('Ctrl Pts',(10.8007906160578,2.44044604391822,3.13621158123827));
#7137=CARTESIAN_POINT('Ctrl Pts',(10.8784706882095,1.13470328440395,4.01476313548051));
#7138=CARTESIAN_POINT('Ctrl Pts',(10.9627400614538,-0.645450738027376,4.01476313548051));
#7139=CARTESIAN_POINT('Ctrl Pts',(11.0172597750513,-1.6320315860502,3.5819951336082));
#7140=CARTESIAN_POINT('Ctrl Pts',(11.0238490761438,-1.74837398213582,3.52379982655521));
#7141=CARTESIAN_POINT('Origin',(11.0238490761438,0.,0.));
#7142=CARTESIAN_POINT('Origin',(11.0238490761438,0.,0.));
#7143=CARTESIAN_POINT('Ctrl Pts',(3.27133852370579,2.84851080212945,2.71166475696575));
#7144=CARTESIAN_POINT('Ctrl Pts',(3.27756781179114,2.76510016696855,2.79918925385792));
#7145=CARTESIAN_POINT('Ctrl Pts',(3.2837527883943,2.67757721529466,2.88281756264117));
#7146=CARTESIAN_POINT('Ctrl Pts',(3.28986642234616,2.5863612587383,2.96220306305726));
#7147=CARTESIAN_POINT('Ctrl Pts',(3.29992445826663,2.43629447770612,3.09280659951976));
#7148=CARTESIAN_POINT('Ctrl Pts',(3.30998041189806,2.2764553229174,3.21217789614563));
#7149=CARTESIAN_POINT('Ctrl Pts',(3.32003847075117,2.10867580690382,3.31906420594094));
#7150=CARTESIAN_POINT('Ctrl Pts',(3.3222082142292,2.07248209239735,3.34212192283809));
#7151=CARTESIAN_POINT('Ctrl Pts',(3.32437805967445,2.03591869476326,3.36459853299068));
#7152=CARTESIAN_POINT('Ctrl Pts',(3.32654805148509,1.99900380615245,3.38648121755032));
#7153=CARTESIAN_POINT('Ctrl Pts',(3.33266414469029,1.89495968105666,3.44815727443238));
#7154=CARTESIAN_POINT('Ctrl Pts',(3.33865883462581,1.78801821896177,3.50493031843278));
#7155=CARTESIAN_POINT('Ctrl Pts',(3.34462164921526,1.67870528210083,3.55662383796714));
#7156=CARTESIAN_POINT('Ctrl Pts',(3.35058846331992,1.56931902436992,3.60835203055972));
#7157=CARTESIAN_POINT('Ctrl Pts',(3.35654216848938,1.45756904643851,3.65502441172559));
#7158=CARTESIAN_POINT('Ctrl Pts',(3.36253222850543,1.343938602328,3.69641849044391));
#7159=CARTESIAN_POINT('Ctrl Pts',(3.36827725878748,1.23495633159455,3.73611930063572));
#7160=CARTESIAN_POINT('Ctrl Pts',(3.37405616830194,1.12424439913972,3.77096467413984));
#7161=CARTESIAN_POINT('Ctrl Pts',(3.37992528781139,1.01225173346125,3.80079224580091));
#7162=CARTESIAN_POINT('Ctrl Pts',(3.37992569942838,1.01224387911722,3.80079433768798));
#7163=CARTESIAN_POINT('Ctrl Pts',(3.37992611104581,1.01223602476688,3.80079642955039));
#7164=CARTESIAN_POINT('Ctrl Pts',(3.37992652266369,1.01222817041023,3.80079852138812));
#7165=CARTESIAN_POINT('Ctrl Pts',(3.38595485692058,0.89719748284113,3.83143445295053));
#7166=CARTESIAN_POINT('Ctrl Pts',(3.39208264801567,0.780693546216728,3.8568063507963));
#7167=CARTESIAN_POINT('Ctrl Pts',(3.39824032428524,0.663227890410915,3.87682699648556));
#7168=CARTESIAN_POINT('Ctrl Pts',(3.40439467936307,0.545825590642329,3.89683684388007));
#7169=CARTESIAN_POINT('Ctrl Pts',(3.41057860191865,0.42746261603,3.9115015228185));
#7170=CARTESIAN_POINT('Ctrl Pts',(3.41674195624578,0.308647273882812,3.92077563304824));
#7171=CARTESIAN_POINT('Ctrl Pts',(3.42290313226368,0.189873924543737,3.93004646553688));
#7172=CARTESIAN_POINT('Ctrl Pts',(3.42904361208695,0.0706467335888831,3.93393067034779));
#7173=CARTESIAN_POINT('Ctrl Pts',(3.43510230316468,-0.0485226577253618,
3.93236313392551));
#7174=CARTESIAN_POINT('Ctrl Pts',(3.44115997878588,-0.167672075858033,3.9307958602275));
#7175=CARTESIAN_POINT('Ctrl Pts',(3.4471804649664,-0.286760773972386,3.92385631726269));
#7176=CARTESIAN_POINT('Ctrl Pts',(3.45320144088977,-0.405304115191476,3.91164518924961));
#7177=CARTESIAN_POINT('Ctrl Pts',(3.45922414139615,-0.523881410678953,3.89943056361352));
#7178=CARTESIAN_POINT('Ctrl Pts',(3.46519339328439,-0.641906978532429,3.88184752285106));
#7179=CARTESIAN_POINT('Ctrl Pts',(3.47110125638993,-0.75886370394298,3.85891687398524));
#7180=CARTESIAN_POINT('Ctrl Pts',(3.47700997128401,-0.875837292032086,3.83598291900633));
#7181=CARTESIAN_POINT('Ctrl Pts',(3.4828863611721,-0.99174991754334,3.80774905124001));
#7182=CARTESIAN_POINT('Ctrl Pts',(3.48877152714845,-1.10610013420366,3.77432248235088));
#7183=CARTESIAN_POINT('Ctrl Pts',(3.49466057807916,-1.22052583647876,3.74087384769593));
#7184=CARTESIAN_POINT('Ctrl Pts',(3.50055873183273,-1.33338691008093,3.70222533306509));
#7185=CARTESIAN_POINT('Ctrl Pts',(3.5065249803474,-1.44418417826052,3.6585283537727));
#7186=CARTESIAN_POINT('Ctrl Pts',(3.50889018855399,-1.48810769356856,3.64120549942439));
#7187=CARTESIAN_POINT('Ctrl Pts',(3.51126626796972,-1.53170691529297,3.62308975173028));
#7188=CARTESIAN_POINT('Ctrl Pts',(3.51365746934456,-1.57495099764014,3.60419264462701));
#7189=CARTESIAN_POINT('Ctrl Pts',(3.51365788148981,-1.57495845115016,3.60418938753912));
#7190=CARTESIAN_POINT('Ctrl Pts',(3.51365829363552,-1.57496590464962,3.60418613042802));
#7191=CARTESIAN_POINT('Ctrl Pts',(3.51365870578167,-1.57497335813855,3.6041828732937));
#7192=CARTESIAN_POINT('Ctrl Pts',(3.51989178432406,-1.68769594777398,3.55492371172874));
#7193=CARTESIAN_POINT('Ctrl Pts',(3.52623092322446,-1.79811199519124,3.50030287918353));
#7194=CARTESIAN_POINT('Ctrl Pts',(3.53260372599692,-1.90574025619246,3.44059439960986));
#7195=CARTESIAN_POINT('Ctrl Pts',(3.53897256246437,-2.0133015315163,3.38092308139987));
#7196=CARTESIAN_POINT('Ctrl Pts',(3.54537469806406,-2.11807877137534,3.31617070281869));
#7197=CARTESIAN_POINT('Ctrl Pts',(3.551757907507,-2.21962094813659,3.24664071361019));
#7198=CARTESIAN_POINT('Ctrl Pts',(3.55813816931474,-2.32111623480328,3.17714283192461));
#7199=CARTESIAN_POINT('Ctrl Pts',(3.56445359556647,-2.41933468255066,3.10280613901885));
#7200=CARTESIAN_POINT('Ctrl Pts',(3.57067623702516,-2.51383508889289,3.02397624789742));
#7201=CARTESIAN_POINT('Ctrl Pts',(3.57838709026876,-2.63093628612604,2.92629333852825));
#7202=CARTESIAN_POINT('Ctrl Pts',(3.58609768658623,-2.74248705096226,2.82190190265532));
#7203=CARTESIAN_POINT('Ctrl Pts',(3.593811064887,-2.84776817148023,2.71146424332989));
#7204=CARTESIAN_POINT('Origin',(11.0238490761438,0.,0.));
#7205=CARTESIAN_POINT('Ctrl Pts',(3.89604095641107,-2.84679354424148,-2.71057216472783));
#7206=CARTESIAN_POINT('Ctrl Pts',(3.92579061605778,-2.44052785873738,-3.13624583529209));
#7207=CARTESIAN_POINT('Ctrl Pts',(4.00347068820956,-1.13491021990779,-4.01486290103005));
#7208=CARTESIAN_POINT('Ctrl Pts',(4.11090042000803,1.13491021990785,-4.01486290102993));
#7209=CARTESIAN_POINT('Ctrl Pts',(4.1885804921598,2.44052785873742,-3.13624583529207));
#7210=CARTESIAN_POINT('Ctrl Pts',(4.21833015180651,2.84679354424151,-2.71057216472779));
#7211=CARTESIAN_POINT('Origin',(11.0238490761438,0.,0.));
#7212=CARTESIAN_POINT('Ctrl Pts',(4.52104095641107,2.84678837447174,2.71057037657591));
#7213=CARTESIAN_POINT('Ctrl Pts',(4.55079061605777,2.44051811330425,3.13624232474605));
#7214=CARTESIAN_POINT('Ctrl Pts',(4.62847068820955,1.13488557063109,4.01485267650142));
#7215=CARTESIAN_POINT('Ctrl Pts',(4.73590042000803,-1.13488557063111,4.01485267650135));
#7216=CARTESIAN_POINT('Ctrl Pts',(4.8135804921598,-2.44051811330426,3.13624232474605));
#7217=CARTESIAN_POINT('Ctrl Pts',(4.84333015180651,-2.84678837447173,2.71057037657592));
#7218=CARTESIAN_POINT('Origin',(11.0238490761438,0.,0.));
#7219=CARTESIAN_POINT('Ctrl Pts',(5.14604095641107,-2.84678351585588,-2.71056863339249));
#7220=CARTESIAN_POINT('Ctrl Pts',(5.17579061605778,-2.44050895442134,-3.13623890248327));
#7221=CARTESIAN_POINT('Ctrl Pts',(5.25347068820956,-1.13486240492507,-4.01484270909931));
#7222=CARTESIAN_POINT('Ctrl Pts',(5.36090042000802,1.13486240492515,-4.01484270909921));
#7223=CARTESIAN_POINT('Ctrl Pts',(5.4385804921598,2.44050895442139,-3.13623890248322));
#7224=CARTESIAN_POINT('Ctrl Pts',(5.46833015180651,2.84678351585592,-2.71056863339245));
#7225=CARTESIAN_POINT('Origin',(11.0238490761438,0.,0.));
#7226=CARTESIAN_POINT('Ctrl Pts',(5.77104095641107,2.84677894112342,2.71056693350226));
#7227=CARTESIAN_POINT('Ctrl Pts',(5.80079061605777,2.44050033068152,3.13623556521482));
#7228=CARTESIAN_POINT('Ctrl Pts',(5.87847068820954,1.13484059276487,4.01483298924472));
#7229=CARTESIAN_POINT('Ctrl Pts',(5.98590042000804,-1.13484059276507,4.01483298924472));
#7230=CARTESIAN_POINT('Ctrl Pts',(6.0635804921598,-2.44050033068153,3.13623556521481));
#7231=CARTESIAN_POINT('Ctrl Pts',(6.0933301518065,-2.84677894112342,2.71056693350226));
#7232=CARTESIAN_POINT('Origin',(11.0238490761438,0.,0.));
#7233=CARTESIAN_POINT('Ctrl Pts',(6.39604095641106,-2.8467746261001,-2.7105652753122));
#7234=CARTESIAN_POINT('Ctrl Pts',(6.42579061605777,-2.44049219651438,-3.13623230981321));
#7235=CARTESIAN_POINT('Ctrl Pts',(6.50347068820954,-1.13482001888854,-4.01482350782885));
#7236=CARTESIAN_POINT('Ctrl Pts',(6.61090042000804,1.13482001888872,-4.01482350782888));
#7237=CARTESIAN_POINT('Ctrl Pts',(6.6885804921598,2.44049219651441,-3.13623230981319));
#7238=CARTESIAN_POINT('Ctrl Pts',(6.71833015180651,2.84677462610012,-2.71056527531218));
#7239=CARTESIAN_POINT('Origin',(11.0238490761438,0.,0.));
#7240=CARTESIAN_POINT('Ctrl Pts',(7.02104095641106,2.84677054928067,2.71056365730649));
#7241=CARTESIAN_POINT('Ctrl Pts',(7.05079061605777,2.4404845113808,3.13622913330255));
#7242=CARTESIAN_POINT('Ctrl Pts',(7.12847068820954,1.13480058075977,4.01481425618423));
#7243=CARTESIAN_POINT('Ctrl Pts',(7.23590042000803,-1.13480058075978,4.01481425618427));
#7244=CARTESIAN_POINT('Ctrl Pts',(7.3135804921598,-2.4404845113808,3.13622913330254));
#7245=CARTESIAN_POINT('Ctrl Pts',(7.34333015180651,-2.84677054928066,2.7105636573065));
#7246=CARTESIAN_POINT('Origin',(11.0238490761438,0.,0.));
#7247=CARTESIAN_POINT('Ctrl Pts',(7.64604095641107,-2.84676669147043,-2.71056207804189));
#7248=CARTESIAN_POINT('Ctrl Pts',(7.67579061605778,-2.44047723909725,-3.1362260328494));
#7249=CARTESIAN_POINT('Ctrl Pts',(7.75347068820955,-1.13478218685908,-4.01480522605852));
#7250=CARTESIAN_POINT('Ctrl Pts',(7.86090042000803,1.13478218685912,-4.01480522605852));
#7251=CARTESIAN_POINT('Ctrl Pts',(7.9385804921598,2.4404772390973,-3.13622603284936));
#7252=CARTESIAN_POINT('Ctrl Pts',(7.96833015180651,2.84676669147048,-2.71056207804184));
#7253=CARTESIAN_POINT('Origin',(11.0238490761438,0.,0.));
#7254=CARTESIAN_POINT('Ctrl Pts',(8.27104095641106,2.84676303548313,2.71056053614337));
#7255=CARTESIAN_POINT('Ctrl Pts',(8.30079061605777,2.44047034726616,3.1362230057544));
#7256=CARTESIAN_POINT('Ctrl Pts',(8.37847068820953,1.13476475524287,4.01479640958965));
#7257=CARTESIAN_POINT('Ctrl Pts',(8.48590042000803,-1.13476475524271,4.01479640958985));
#7258=CARTESIAN_POINT('Ctrl Pts',(8.56358049215979,-2.44047034726616,3.1362230057544));
#7259=CARTESIAN_POINT('Ctrl Pts',(8.59333015180651,-2.84676303548312,2.71056053614338));
#7260=CARTESIAN_POINT('Origin',(11.0238490761438,0.,0.));
#7261=CARTESIAN_POINT('Ctrl Pts',(8.89604095641106,-2.84675956588473,-2.71055903030038));
#7262=CARTESIAN_POINT('Ctrl Pts',(8.92579061605777,-2.44046380679322,-3.1362200494445));
#7263=CARTESIAN_POINT('Ctrl Pts',(9.00347068820953,-1.13474821232218,-4.01478779928378));
#7264=CARTESIAN_POINT('Ctrl Pts',(9.11090042000803,1.13474821232205,-4.01478779928393));
#7265=CARTESIAN_POINT('Ctrl Pts',(9.18858049215979,2.44046380679323,-3.1362200494445));
#7266=CARTESIAN_POINT('Ctrl Pts',(9.21833015180651,2.84675956588473,-2.71055903030039));
#7267=CARTESIAN_POINT('Origin',(11.0238490761438,0.,0.));
#7268=CARTESIAN_POINT('Ctrl Pts',(9.52104095641107,2.84675626877589,2.71055755926284));
#7269=CARTESIAN_POINT('Ctrl Pts',(9.55079061605777,2.44045759147703,3.13621716146554));
#7270=CARTESIAN_POINT('Ctrl Pts',(9.62847068820954,1.1347324918254,4.01477938799309));
#7271=CARTESIAN_POINT('Ctrl Pts',(9.73590042000802,-1.13473249182541,4.01477938799308));
#7272=CARTESIAN_POINT('Ctrl Pts',(9.81358049215979,-2.44045759147703,3.13621716146554));
#7273=CARTESIAN_POINT('Ctrl Pts',(9.84333015180651,-2.84675626877588,2.71055755926285));
#7274=CARTESIAN_POINT('Origin',(11.0238490761438,0.,0.));
#7275=CARTESIAN_POINT('Ctrl Pts',(10.1460409564111,-2.84675313160574,-2.7105561218378));
#7276=CARTESIAN_POINT('Ctrl Pts',(10.1757906160578,-2.44045167765816,-3.13621433947552));
#7277=CARTESIAN_POINT('Ctrl Pts',(10.2534706882095,-1.13471753391067,-4.01477116889627));
#7278=CARTESIAN_POINT('Ctrl Pts',(10.360900420008,1.13471753391068,-4.01477116889624));
#7279=CARTESIAN_POINT('Ctrl Pts',(10.4385804921598,2.44045167765817,-3.13621433947552));
#7280=CARTESIAN_POINT('Ctrl Pts',(10.4683301518065,2.84675313160573,-2.71055612183781));
#7281=CARTESIAN_POINT('Ctrl Pts',(4.27290740952806,3.47674578943201,-1.83867552770464));
#7282=CARTESIAN_POINT('Ctrl Pts',(4.22496533064083,3.03366144096162,-2.67651685389203));
#7283=CARTESIAN_POINT('Ctrl Pts',(4.12909283924855,1.51928728527458,-4.01486290102995));
#7284=CARTESIAN_POINT('Ctrl Pts',(3.98527826896903,-1.51928728527452,-4.01486290102998));
#7285=CARTESIAN_POINT('Ctrl Pts',(3.88940577757674,-3.03366144096159,-2.67651685389207));
#7286=CARTESIAN_POINT('Ctrl Pts',(3.84146369868952,-3.47674578943198,-1.8386755277047));
#7287=CARTESIAN_POINT('Ctrl Pts',(4.13588920451707,3.26695428751823,-1.72772738140596));
#7288=CARTESIAN_POINT('Ctrl Pts',(4.08794712562984,2.85060624264031,-2.51501223874808));
#7289=CARTESIAN_POINT('Ctrl Pts',(3.99207463423756,1.42761145370095,-3.7726006911942));
#7290=CARTESIAN_POINT('Ctrl Pts',(3.84826006395804,-1.42761145370091,-3.77260069119421));
#7291=CARTESIAN_POINT('Ctrl Pts',(3.75238757256575,-2.85060624264028,-2.51501223874812));
#7292=CARTESIAN_POINT('Ctrl Pts',(3.70444549367851,-3.26695428751821,-1.72772738140599));
#7293=CARTESIAN_POINT('Ctrl Pts',(3.99887099950606,3.05716278560445,-1.61677923510726));
#7294=CARTESIAN_POINT('Ctrl Pts',(3.95092892061883,2.667551044319,-2.35350762360415));
#7295=CARTESIAN_POINT('Ctrl Pts',(3.85505642922655,1.33593562212733,-3.53033848135843));
#7296=CARTESIAN_POINT('Ctrl Pts',(3.71124185894703,-1.3359356221273,-3.53033848135844));
#7297=CARTESIAN_POINT('Ctrl Pts',(3.61536936755474,-2.66755104431898,-2.35350762360417));
#7298=CARTESIAN_POINT('Ctrl Pts',(3.56742728866751,-3.05716278560443,-1.61677923510729));
#7299=CARTESIAN_POINT('Ctrl Pts',(3.86185279449507,2.84737128369067,-1.50583108880857));
#7300=CARTESIAN_POINT('Ctrl Pts',(3.81391071560784,2.48449584599769,-2.19200300846021));
#7301=CARTESIAN_POINT('Ctrl Pts',(3.71803822421555,1.2442597905537,-3.28807627152267));
#7302=CARTESIAN_POINT('Ctrl Pts',(3.57422365393604,-1.24425979055368,-3.28807627152268));
#7303=CARTESIAN_POINT('Ctrl Pts',(3.47835116254375,-2.48449584599768,-2.19200300846022));
#7304=CARTESIAN_POINT('Ctrl Pts',(3.43040908365653,-2.84737128369066,-1.50583108880859));
#7305=CARTESIAN_POINT('Ctrl Pts',(5.52290755913492,3.47674717210332,-1.83867291315533));
#7306=CARTESIAN_POINT('Ctrl Pts',(5.47496543037874,3.03366303203899,-2.67651546652179));
#7307=CARTESIAN_POINT('Ctrl Pts',(5.3790928891175,1.51922432968233,-4.01484270909923));
#7308=CARTESIAN_POINT('Ctrl Pts',(5.23527821910008,-1.51922432968225,-4.01484270909927));
#7309=CARTESIAN_POINT('Ctrl Pts',(5.13940567783883,-3.03366303203894,-2.67651546652185));
#7310=CARTESIAN_POINT('Ctrl Pts',(5.09146354908265,-3.47674717210328,-1.83867291315541));
#7311=CARTESIAN_POINT('Ctrl Pts',(5.38589301138905,3.26696118647632,-1.72772788602568));
#7312=CARTESIAN_POINT('Ctrl Pts',(5.33795088263287,2.85061262378872,-2.51501524594334));
#7313=CARTESIAN_POINT('Ctrl Pts',(5.24207834137162,1.42755474382685,-3.77258818405817));
#7314=CARTESIAN_POINT('Ctrl Pts',(5.0982636713542,-1.42755474382678,-3.7725881840582));
#7315=CARTESIAN_POINT('Ctrl Pts',(5.00239113009296,-2.85061262378867,-2.5150152459434));
#7316=CARTESIAN_POINT('Ctrl Pts',(4.95444900133677,-3.26696118647629,-1.72772788602574));
#7317=CARTESIAN_POINT('Ctrl Pts',(5.24887846364316,3.05717520084931,-1.61678285889602));
#7318=CARTESIAN_POINT('Ctrl Pts',(5.20093633488698,2.66756221553844,-2.3535150253649));
#7319=CARTESIAN_POINT('Ctrl Pts',(5.10506379362574,1.33588515797135,-3.5303336590171));
#7320=CARTESIAN_POINT('Ctrl Pts',(4.96124912360832,-1.3358851579713,-3.53033365901712));
#7321=CARTESIAN_POINT('Ctrl Pts',(4.86537658234707,-2.6675622155384,-2.35351502536494));
#7322=CARTESIAN_POINT('Ctrl Pts',(4.81743445359089,-3.05717520084929,-1.61678285889607));
#7323=CARTESIAN_POINT('Ctrl Pts',(5.11186391589729,2.84738921522231,-1.50583783176637));
#7324=CARTESIAN_POINT('Ctrl Pts',(5.06392178714111,2.48451180728816,-2.19201480478645));
#7325=CARTESIAN_POINT('Ctrl Pts',(4.96804924587987,1.24421557211587,-3.28807913397604));
#7326=CARTESIAN_POINT('Ctrl Pts',(4.82423457586244,-1.24421557211583,-3.28807913397605));
#7327=CARTESIAN_POINT('Ctrl Pts',(4.7283620346012,-2.48451180728813,-2.19201480478648));
#7328=CARTESIAN_POINT('Ctrl Pts',(4.68041990584502,-2.84738921522229,-1.50583783176641));
#7329=CARTESIAN_POINT('Ctrl Pts',(6.77290769409362,3.47674841939408,-1.83867055459827));
#7330=CARTESIAN_POINT('Ctrl Pts',(6.72496552035121,3.03366446720085,-2.67651421526794));
#7331=CARTESIAN_POINT('Ctrl Pts',(6.62909293410373,1.51916853850403,-4.01482350782886));
#7332=CARTESIAN_POINT('Ctrl Pts',(6.48527817411384,-1.51916853850395,-4.01482350782889));
#7333=CARTESIAN_POINT('Ctrl Pts',(6.38940558786636,-3.0336644672008,-2.676514215268));
#7334=CARTESIAN_POINT('Ctrl Pts',(6.34146341412395,-3.47674841939404,-1.83867055459834));
#7335=CARTESIAN_POINT('Ctrl Pts',(6.63589656027986,3.26696758565425,-1.72772843414892));
#7336=CARTESIAN_POINT('Ctrl Pts',(6.58795438653744,2.85061853334314,-2.51501809421893));
#7337=CARTESIAN_POINT('Ctrl Pts',(6.49208180028997,1.42750460308064,-3.7725761775094));
#7338=CARTESIAN_POINT('Ctrl Pts',(6.34826704030007,-1.42750460308057,-3.77257617750942));
#7339=CARTESIAN_POINT('Ctrl Pts',(6.25239445405259,-2.85061853334309,-2.51501809421899));
#7340=CARTESIAN_POINT('Ctrl Pts',(6.20445228031018,-3.26696758565422,-1.72772843414898));
#7341=CARTESIAN_POINT('Ctrl Pts',(6.49888542646609,3.05718675191442,-1.61678631369958));
#7342=CARTESIAN_POINT('Ctrl Pts',(6.45094325272367,2.66757259948543,-2.35352197316993));
#7343=CARTESIAN_POINT('Ctrl Pts',(6.35507066647619,1.33584066765725,-3.53032884718994));
#7344=CARTESIAN_POINT('Ctrl Pts',(6.2112559064863,-1.3358406676572,-3.53032884718996));
#7345=CARTESIAN_POINT('Ctrl Pts',(6.11538332023882,-2.66757259948539,-2.35352197316997));
#7346=CARTESIAN_POINT('Ctrl Pts',(6.0674411464964,-3.0571867519144,-1.61678631369962));
#7347=CARTESIAN_POINT('Ctrl Pts',(6.36187429265231,2.84740591817458,-1.50584419325024));
#7348=CARTESIAN_POINT('Ctrl Pts',(6.3139321189099,2.48452666562772,-2.19202585212091));
#7349=CARTESIAN_POINT('Ctrl Pts',(6.21805953266242,1.24417673223386,-3.28808151687049));
#7350=CARTESIAN_POINT('Ctrl Pts',(6.07424477267253,-1.24417673223382,-3.28808151687051));
#7351=CARTESIAN_POINT('Ctrl Pts',(5.97837218642505,-2.4845266656277,-2.19202585212095));
#7352=CARTESIAN_POINT('Ctrl Pts',(5.93043001268264,-2.84740591817456,-1.50584419325028));
#7353=CARTESIAN_POINT('Ctrl Pts',(8.02290781660591,3.47674955165342,-1.83866841355563));
#7354=CARTESIAN_POINT('Ctrl Pts',(7.97496560202607,3.03366576988594,-2.67651307964991));
#7355=CARTESIAN_POINT('Ctrl Pts',(7.87909297494116,1.51911875599997,-4.01480522605851));
#7356=CARTESIAN_POINT('Ctrl Pts',(7.73527813327642,-1.51911875599992,-4.01480522605853));
#7357=CARTESIAN_POINT('Ctrl Pts',(7.6394055061915,-3.03366576988591,-2.67651307964995));
#7358=CARTESIAN_POINT('Ctrl Pts',(7.59146329161166,-3.4767495516534,-1.83866841355567));
#7359=CARTESIAN_POINT('Ctrl Pts',(7.88589988091443,3.26697354631375,-1.72772901190777));
#7360=CARTESIAN_POINT('Ctrl Pts',(7.83795766633459,2.85062403009778,-2.51502079677286));
#7361=CARTESIAN_POINT('Ctrl Pts',(7.74208503924968,1.42745996391967,-3.77256465335495));
#7362=CARTESIAN_POINT('Ctrl Pts',(7.59827019758493,-1.42745996391964,-3.77256465335497));
#7363=CARTESIAN_POINT('Ctrl Pts',(7.50239757050003,-2.85062403009776,-2.51502079677288));
#7364=CARTESIAN_POINT('Ctrl Pts',(7.45445535592019,-3.26697354631373,-1.7277290119078));
#7365=CARTESIAN_POINT('Ctrl Pts',(7.74889194522295,3.05719754097409,-1.61678961025991));
#7366=CARTESIAN_POINT('Ctrl Pts',(7.7009497306431,2.66758229030962,-2.35352851389579));
#7367=CARTESIAN_POINT('Ctrl Pts',(7.6050771035582,1.33580117183938,-3.5303240806514));
#7368=CARTESIAN_POINT('Ctrl Pts',(7.46126226189346,-1.33580117183935,-3.53032408065141));
#7369=CARTESIAN_POINT('Ctrl Pts',(7.36538963480854,-2.6675822903096,-2.35352851389581));
#7370=CARTESIAN_POINT('Ctrl Pts',(7.3174474202287,-3.05719754097408,-1.61678961025993));
#7371=CARTESIAN_POINT('Ctrl Pts',(7.61188400953148,2.84742153563442,-1.50585020861204));
#7372=CARTESIAN_POINT('Ctrl Pts',(7.56394179495163,2.48454055052145,-2.19203623101873));
#7373=CARTESIAN_POINT('Ctrl Pts',(7.46806916786671,1.24414237975909,-3.28808350794784));
#7374=CARTESIAN_POINT('Ctrl Pts',(7.32425432620197,-1.24414237975908,-3.28808350794785));
#7375=CARTESIAN_POINT('Ctrl Pts',(7.22838169911706,-2.48454055052144,-2.19203623101874));
#7376=CARTESIAN_POINT('Ctrl Pts',(7.18043948453722,-2.84742153563441,-1.50585020861206));
#7377=CARTESIAN_POINT('Ctrl Pts',(9.27290792843865,3.47675058521116,-1.83866645914951));
#7378=CARTESIAN_POINT('Ctrl Pts',(9.22496567658123,3.03366695890456,-2.67651204323431));
#7379=CARTESIAN_POINT('Ctrl Pts',(9.12909301221873,1.51907406221497,-4.01478779928389));
#7380=CARTESIAN_POINT('Ctrl Pts',(8.98527809599884,-1.51907406221493,-4.0147877992839));
#7381=CARTESIAN_POINT('Ctrl Pts',(8.88940543163634,-3.03366695890454,-2.67651204323434));
#7382=CARTESIAN_POINT('Ctrl Pts',(8.84146317977892,-3.47675058521115,-1.83866645914954));
#7383=CARTESIAN_POINT('Ctrl Pts',(9.13590299800969,3.26697911893791,-1.72772960887218));
#7384=CARTESIAN_POINT('Ctrl Pts',(9.08796074615226,2.85062916238817,-2.51502336521541));
#7385=CARTESIAN_POINT('Ctrl Pts',(8.99208808178978,1.42741997728753,-3.77255359156877));
#7386=CARTESIAN_POINT('Ctrl Pts',(8.84827316556986,-1.4274199772875,-3.77255359156878));
#7387=CARTESIAN_POINT('Ctrl Pts',(8.75240050120738,-2.85062916238816,-2.51502336521541));
#7388=CARTESIAN_POINT('Ctrl Pts',(8.70445824934996,-3.2669791189379,-1.72772960887219));
#7389=CARTESIAN_POINT('Ctrl Pts',(8.99889806758071,3.05720765266466,-1.61679275859484));
#7390=CARTESIAN_POINT('Ctrl Pts',(8.95095581572329,2.66759136587177,-2.35353468719648));
#7391=CARTESIAN_POINT('Ctrl Pts',(8.85508315136081,1.33576589236007,-3.53031938385365));
#7392=CARTESIAN_POINT('Ctrl Pts',(8.71126823514089,-1.33576589236006,-3.53031938385365));
#7393=CARTESIAN_POINT('Ctrl Pts',(8.61539557077841,-2.66759136587176,-2.35353468719649));
#7394=CARTESIAN_POINT('Ctrl Pts',(8.56745331892098,-3.05720765266466,-1.61679275859485));
#7395=CARTESIAN_POINT('Ctrl Pts',(8.86189313715175,2.84743618639142,-1.5058559083175));
#7396=CARTESIAN_POINT('Ctrl Pts',(8.81395088529433,2.48455356935539,-2.19204600917757));
#7397=CARTESIAN_POINT('Ctrl Pts',(8.71807822093185,1.24411180743262,-3.28808517613852));
#7398=CARTESIAN_POINT('Ctrl Pts',(8.57426330471193,-1.24411180743262,-3.28808517613852));
#7399=CARTESIAN_POINT('Ctrl Pts',(8.47839064034944,-2.48455356935539,-2.19204600917757));
#7400=CARTESIAN_POINT('Ctrl Pts',(8.43044838849202,-2.84743618639142,-1.5058559083175));
#7401=CARTESIAN_POINT('Ctrl Pts',(10.5229080310278,3.47675153333854,-1.83866466628547));
#7402=CARTESIAN_POINT('Ctrl Pts',(10.474965744974,3.03366804954435,-2.67651109266735));
#7403=CARTESIAN_POINT('Ctrl Pts',(10.3790930464151,1.51903371577996,-4.01477116889625));
#7404=CARTESIAN_POINT('Ctrl Pts',(10.2352780618025,-1.51903371577993,-4.01477116889626));
#7405=CARTESIAN_POINT('Ctrl Pts',(10.1394053632436,-3.03366804954433,-2.67651109266738));
#7406=CARTESIAN_POINT('Ctrl Pts',(10.0914630771898,-3.47675153333853,-1.8386646662855));
#7407=CARTESIAN_POINT('Ctrl Pts',(10.3859059323742,3.26698434565854,-1.72773021714958));
#7408=CARTESIAN_POINT('Ctrl Pts',(10.3379636463205,2.85063397046062,-2.51502580983381));
#7409=CARTESIAN_POINT('Ctrl Pts',(10.2420909477615,1.4273839595363,-3.77254297133811));
#7410=CARTESIAN_POINT('Ctrl Pts',(10.0982759631489,-1.42738395953627,-3.77254297133812));
#7411=CARTESIAN_POINT('Ctrl Pts',(10.00240326459,-2.85063397046061,-2.51502580983382));
#7412=CARTESIAN_POINT('Ctrl Pts',(9.95446097853621,-3.26698434565853,-1.7277302171496));
#7413=CARTESIAN_POINT('Ctrl Pts',(10.2489038337206,3.05721715797854,-1.61679576801369));
#7414=CARTESIAN_POINT('Ctrl Pts',(10.2009615476668,2.66759989137687,-2.35354052700025));
#7415=CARTESIAN_POINT('Ctrl Pts',(10.105088849108,1.33573420329263,-3.53031477377997));
#7416=CARTESIAN_POINT('Ctrl Pts',(9.96127386449531,-1.33573420329262,-3.53031477377997));
#7417=CARTESIAN_POINT('Ctrl Pts',(9.86540116593643,-2.66759989137686,-2.35354052700027));
#7418=CARTESIAN_POINT('Ctrl Pts',(9.81745887988263,-3.05721715797854,-1.6167957680137));
#7419=CARTESIAN_POINT('Ctrl Pts',(10.111901735067,2.84744997029854,-1.5058613188778));
#7420=CARTESIAN_POINT('Ctrl Pts',(10.0639594490133,2.48456581229314,-2.19205524416672));
#7421=CARTESIAN_POINT('Ctrl Pts',(9.96808675045439,1.24408444704895,-3.28808657622182));
#7422=CARTESIAN_POINT('Ctrl Pts',(9.82427176584173,-1.24408444704895,-3.28808657622182));
#7423=CARTESIAN_POINT('Ctrl Pts',(9.72839906728286,-2.48456581229314,-2.19205524416672));
#7424=CARTESIAN_POINT('Ctrl Pts',(9.68045678122906,-2.84744997029854,-1.5058613188778));
#7425=CARTESIAN_POINT('Ctrl Pts',(3.64838128925859,-3.47740286631016,1.83922164452567));
#7426=CARTESIAN_POINT('Ctrl Pts',(3.60379518879799,-3.06521053407891,2.61855938315106));
#7427=CARTESIAN_POINT('Ctrl Pts',(3.51463169441755,-1.69992623500153,3.88752819359771));
#7428=CARTESIAN_POINT('Ctrl Pts',(3.38089080611729,1.09279645395022,4.09974510230776));
#7429=CARTESIAN_POINT('Ctrl Pts',(3.29173601827763,2.63403351313429,3.0518682259016));
#7430=CARTESIAN_POINT('Ctrl Pts',(3.24715862435781,3.1592487603224,2.34397402547678));
#7431=CARTESIAN_POINT('Ctrl Pts',(3.51131387403993,-3.26754097150884,1.72822428410498));
#7432=CARTESIAN_POINT('Ctrl Pts',(3.46672777357933,-2.88022452142018,2.46052884860418));
#7433=CARTESIAN_POINT('Ctrl Pts',(3.37756427919888,-1.59733537785462,3.65291516077772));
#7434=CARTESIAN_POINT('Ctrl Pts',(3.24382339089863,1.02684598940094,3.85232474048881));
#7435=CARTESIAN_POINT('Ctrl Pts',(3.15466860305897,2.47506911203139,2.86768742396558));
#7436=CARTESIAN_POINT('Ctrl Pts',(3.11009120913914,2.9685875236238,2.20251476715576));
#7437=CARTESIAN_POINT('Ctrl Pts',(3.37424645882128,-3.05767907670752,1.61722692368431));
#7438=CARTESIAN_POINT('Ctrl Pts',(3.32966035836067,-2.69523850876146,2.30249831405731));
#7439=CARTESIAN_POINT('Ctrl Pts',(3.24049686398023,-1.4947445207077,3.41830212795774));
#7440=CARTESIAN_POINT('Ctrl Pts',(3.10675597567997,0.960895524851675,3.60490437866986));
#7441=CARTESIAN_POINT('Ctrl Pts',(3.01760118784032,2.31610471092849,2.68350662202955));
#7442=CARTESIAN_POINT('Ctrl Pts',(2.97302379392049,2.77792628692519,2.06105550883474));
#7443=CARTESIAN_POINT('Ctrl Pts',(3.23717904360261,-2.84781718190621,1.50622956326363));
#7444=CARTESIAN_POINT('Ctrl Pts',(3.192592943142,-2.51025249610272,2.14446777951043));
#7445=CARTESIAN_POINT('Ctrl Pts',(3.10342944876156,-1.39215366356079,3.18368909513775));
#7446=CARTESIAN_POINT('Ctrl Pts',(2.96968856046131,0.8949450603024,3.35748401685091));
#7447=CARTESIAN_POINT('Ctrl Pts',(2.88053377262165,2.15714030982559,2.49932582009352));
#7448=CARTESIAN_POINT('Ctrl Pts',(2.83595637870183,2.5872650502266,1.91959625051372));
#7449=CARTESIAN_POINT('Ctrl Pts',(4.89790748632074,-3.47674649915261,1.83867418566579));
#7450=CARTESIAN_POINT('Ctrl Pts',(4.84996538183595,-3.03366225767408,2.67651614172047));
#7451=CARTESIAN_POINT('Ctrl Pts',(4.7540928648461,-1.51925482848182,4.01485267650136));
#7452=CARTESIAN_POINT('Ctrl Pts',(4.61027824337146,1.51925482848179,4.01485267650137));
#7453=CARTESIAN_POINT('Ctrl Pts',(4.51440572638162,3.03366225767406,2.67651614172049));
#7454=CARTESIAN_POINT('Ctrl Pts',(4.46646362189683,3.47674649915259,1.83867418566581));
#7455=CARTESIAN_POINT('Ctrl Pts',(4.76089114229214,-3.26695780380383,1.72772762724506));
#7456=CARTESIAN_POINT('Ctrl Pts',(4.71294903780735,-2.85060949632914,2.51501376310635));
#7457=CARTESIAN_POINT('Ctrl Pts',(4.6170765208175,-1.42758220050988,3.77259437402633));
#7458=CARTESIAN_POINT('Ctrl Pts',(4.47326189934286,1.42758220050987,3.77259437402634));
#7459=CARTESIAN_POINT('Ctrl Pts',(4.37738938235302,2.85060949632913,2.51501376310635));
#7460=CARTESIAN_POINT('Ctrl Pts',(4.32944727786822,3.26695780380383,1.72772762724508));
#7461=CARTESIAN_POINT('Ctrl Pts',(4.62387479826355,-3.05716910845506,1.61678106882435));
#7462=CARTESIAN_POINT('Ctrl Pts',(4.57593269377875,-2.66755673498418,2.35351138449224));
#7463=CARTESIAN_POINT('Ctrl Pts',(4.48006017678891,-1.33590957253795,3.5303360715513));
#7464=CARTESIAN_POINT('Ctrl Pts',(4.33624555531426,1.33590957253794,3.5303360715513));
#7465=CARTESIAN_POINT('Ctrl Pts',(4.24037303832442,2.66755673498418,2.35351138449224));
#7466=CARTESIAN_POINT('Ctrl Pts',(4.19243093383963,3.05716910845506,1.61678106882436));
#7467=CARTESIAN_POINT('Ctrl Pts',(4.48685845423494,-2.8473804131063,1.50583451040362));
#7468=CARTESIAN_POINT('Ctrl Pts',(4.43891634975015,-2.48450397363924,2.19200900587812));
#7469=CARTESIAN_POINT('Ctrl Pts',(4.34304383276031,-1.24423694456603,3.28807776907627));
#7470=CARTESIAN_POINT('Ctrl Pts',(4.19922921128567,1.24423694456603,3.28807776907627));
#7471=CARTESIAN_POINT('Ctrl Pts',(4.10335669429582,2.48450397363925,2.19200900587812));
#7472=CARTESIAN_POINT('Ctrl Pts',(4.05541458981104,2.84738041310631,1.50583451040362));
#7473=CARTESIAN_POINT('Ctrl Pts',(6.14790762829603,-3.47674781129169,1.8386717044864));
#7474=CARTESIAN_POINT('Ctrl Pts',(6.09996547648614,-3.03366376752034,2.67651482526888));
#7475=CARTESIAN_POINT('Ctrl Pts',(6.0040929121712,-1.51919561710872,4.01483298924471));
#7476=CARTESIAN_POINT('Ctrl Pts',(5.86027819604637,1.51919561710867,4.01483298924473));
#7477=CARTESIAN_POINT('Ctrl Pts',(5.76440563173143,3.03366376752031,2.67651482526892));
#7478=CARTESIAN_POINT('Ctrl Pts',(5.71646347992155,3.47674781129167,1.83867170448645));
#7479=CARTESIAN_POINT('Ctrl Pts',(6.01089481609153,-3.26696444442227,1.72772815560951));
#7480=CARTESIAN_POINT('Ctrl Pts',(5.96295266428165,-2.85061563356214,2.51501668908045));
#7481=CARTESIAN_POINT('Ctrl Pts',(5.8670800999667,-1.42752892490422,3.77258211928897));
#7482=CARTESIAN_POINT('Ctrl Pts',(5.72326538384188,1.42752892490418,3.77258211928898));
#7483=CARTESIAN_POINT('Ctrl Pts',(5.62739281952693,2.85061563356211,2.51501668908049));
#7484=CARTESIAN_POINT('Ctrl Pts',(5.57945066771705,3.26696444442225,1.72772815560954));
#7485=CARTESIAN_POINT('Ctrl Pts',(5.87388200388703,-3.05718107755285,1.61678460673262));
#7486=CARTESIAN_POINT('Ctrl Pts',(5.82593985207715,-2.66756749960396,2.35351855289203));
#7487=CARTESIAN_POINT('Ctrl Pts',(5.73006728776221,-1.33586223269973,3.53033124933322));
#7488=CARTESIAN_POINT('Ctrl Pts',(5.58625257163737,1.3358622326997,3.53033124933323));
#7489=CARTESIAN_POINT('Ctrl Pts',(5.49038000732244,2.66756749960394,2.35351855289205));
#7490=CARTESIAN_POINT('Ctrl Pts',(5.44243785551255,3.05718107755284,1.61678460673264));
#7491=CARTESIAN_POINT('Ctrl Pts',(5.73686919168254,-2.84739771068344,1.50584105785573));
#7492=CARTESIAN_POINT('Ctrl Pts',(5.68892703987265,-2.48451936564576,2.19202041670361));
#7493=CARTESIAN_POINT('Ctrl Pts',(5.59305447555771,-1.24419554049523,3.28808037937748));
#7494=CARTESIAN_POINT('Ctrl Pts',(5.44923975943288,1.24419554049521,3.28808037937748));
#7495=CARTESIAN_POINT('Ctrl Pts',(5.35336719511794,2.48451936564575,2.19202041670362));
#7496=CARTESIAN_POINT('Ctrl Pts',(5.30542504330806,2.84739771068344,1.50584105785575));
#7497=CARTESIAN_POINT('Ctrl Pts',(7.39790775678633,-3.47674899880063,1.83866945897147));
#7498=CARTESIAN_POINT('Ctrl Pts',(7.34996556214635,-3.03366513383357,2.67651363411353));
#7499=CARTESIAN_POINT('Ctrl Pts',(7.2540929550013,-1.51914295842827,4.01481425618425));
#7500=CARTESIAN_POINT('Ctrl Pts',(7.11027815321627,1.51914295842826,4.01481425618426));
#7501=CARTESIAN_POINT('Ctrl Pts',(7.01440554607122,3.03366513383357,2.67651363411354));
#7502=CARTESIAN_POINT('Ctrl Pts',(6.96646335143124,3.47674899880063,1.83866945897148));
#7503=CARTESIAN_POINT('Ctrl Pts',(7.26089824748156,-3.26697061742319,1.72772872004433));
#7504=CARTESIAN_POINT('Ctrl Pts',(7.21295605284158,-2.85062133008578,2.5150194629517));
#7505=CARTESIAN_POINT('Ctrl Pts',(7.11708344569652,-1.42748165328085,3.772570356356));
#7506=CARTESIAN_POINT('Ctrl Pts',(6.9732686439115,1.42748165328084,3.77257035635601));
#7507=CARTESIAN_POINT('Ctrl Pts',(6.87739603676645,2.85062133008577,2.51501946295171));
#7508=CARTESIAN_POINT('Ctrl Pts',(6.82945384212647,3.26697061742319,1.72772872004433));
#7509=CARTESIAN_POINT('Ctrl Pts',(7.12388873817679,-3.05719223604573,1.61678798111718));
#7510=CARTESIAN_POINT('Ctrl Pts',(7.07594654353681,-2.66757752633796,2.35352529178989));
#7511=CARTESIAN_POINT('Ctrl Pts',(6.98007393639176,-1.33582034813344,3.53032645652775));
#7512=CARTESIAN_POINT('Ctrl Pts',(6.83625913460674,1.33582034813344,3.53032645652775));
#7513=CARTESIAN_POINT('Ctrl Pts',(6.74038652746168,2.66757752633797,2.35352529178988));
#7514=CARTESIAN_POINT('Ctrl Pts',(6.6924443328217,3.05719223604573,1.61678798111717));
#7515=CARTESIAN_POINT('Ctrl Pts',(6.98687922887202,-2.84741385466828,1.50584724219002));
#7516=CARTESIAN_POINT('Ctrl Pts',(6.93893703423204,-2.48453372259017,2.19203112062806));
#7517=CARTESIAN_POINT('Ctrl Pts',(6.84306442708698,-1.24415904298601,3.28808255669949));
#7518=CARTESIAN_POINT('Ctrl Pts',(6.69924962530196,1.24415904298602,3.28808255669949));
#7519=CARTESIAN_POINT('Ctrl Pts',(6.60337701815691,2.48453372259019,2.19203112062805));
#7520=CARTESIAN_POINT('Ctrl Pts',(6.55543482351693,2.84741385466829,1.50584724219001));
#7521=CARTESIAN_POINT('Ctrl Pts',(8.64790787376072,-3.47675007987806,1.83866741470954));
#7522=CARTESIAN_POINT('Ctrl Pts',(8.59996564012927,-3.03366637757612,2.67651254993933));
#7523=CARTESIAN_POINT('Ctrl Pts',(8.50409299399277,-1.51909582299121,4.01479640958979));
#7524=CARTESIAN_POINT('Ctrl Pts',(8.3602781142248,1.51909582299119,4.0147964095898));
#7525=CARTESIAN_POINT('Ctrl Pts',(8.2644054680883,3.03366637757611,2.67651254993935));
#7526=CARTESIAN_POINT('Ctrl Pts',(8.21646323445685,3.47675007987805,1.83866741470956));
#7527=CARTESIAN_POINT('Ctrl Pts',(8.51090146352299,-3.26697637832471,1.72772930853349));
#7528=CARTESIAN_POINT('Ctrl Pts',(8.46295922989154,-2.85062663911888,2.51502209708675));
#7529=CARTESIAN_POINT('Ctrl Pts',(8.36708658375503,-1.42743943513422,3.77255906595759));
#7530=CARTESIAN_POINT('Ctrl Pts',(8.22327170398708,1.42743943513421,3.77255906595759));
#7531=CARTESIAN_POINT('Ctrl Pts',(8.12739905785057,2.85062663911887,2.51502209708676));
#7532=CARTESIAN_POINT('Ctrl Pts',(8.07945682421912,3.26697637832471,1.7277293085335));
#7533=CARTESIAN_POINT('Ctrl Pts',(8.37389505328524,-3.05720267677136,1.61679120235743));
#7534=CARTESIAN_POINT('Ctrl Pts',(8.32595281965381,-2.66758690066164,2.35353164423417));
#7535=CARTESIAN_POINT('Ctrl Pts',(8.23008017351729,-1.33578304727724,3.53032172232538));
#7536=CARTESIAN_POINT('Ctrl Pts',(8.08626529374934,1.33578304727724,3.53032172232538));
#7537=CARTESIAN_POINT('Ctrl Pts',(7.99039264761284,2.66758690066164,2.35353164423417));
#7538=CARTESIAN_POINT('Ctrl Pts',(7.94245041398138,3.05720267677136,1.61679120235743));
#7539=CARTESIAN_POINT('Ctrl Pts',(8.23688864304753,-2.84742897521801,1.50585309618137));
#7540=CARTESIAN_POINT('Ctrl Pts',(8.18894640941607,-2.48454716220439,2.1920411913816));
#7541=CARTESIAN_POINT('Ctrl Pts',(8.09307376327956,-1.24412665942025,3.28808437869317));
#7542=CARTESIAN_POINT('Ctrl Pts',(7.94925888351161,1.24412665942026,3.28808437869317));
#7543=CARTESIAN_POINT('Ctrl Pts',(7.85338623737511,2.4845471622044,2.19204119138159));
#7544=CARTESIAN_POINT('Ctrl Pts',(7.80544400374366,2.84742897521802,1.50585309618137));
#7545=CARTESIAN_POINT('Ctrl Pts',(9.89790798080964,-3.47675106922323,1.83866554390586));
#7546=CARTESIAN_POINT('Ctrl Pts',(9.84996571149522,-3.0336675156804,2.67651155795465));
#7547=CARTESIAN_POINT('Ctrl Pts',(9.75409302967573,-1.51905338615236,4.01477938799308));
#7548=CARTESIAN_POINT('Ctrl Pts',(9.61027807854184,1.51905338615236,4.01477938799308));
#7549=CARTESIAN_POINT('Ctrl Pts',(9.51440539672235,3.0336675156804,2.67651155795466));
#7550=CARTESIAN_POINT('Ctrl Pts',(9.46646312740793,3.47675106922323,1.83866554390586));
#7551=CARTESIAN_POINT('Ctrl Pts',(9.76090448686174,-3.26698177317707,1.72772991200983));
#7552=CARTESIAN_POINT('Ctrl Pts',(9.71296221754732,-2.85063160470143,2.51502460240538));
#7553=CARTESIAN_POINT('Ctrl Pts',(9.61708953572784,-1.42740150969491,3.77254822757006));
#7554=CARTESIAN_POINT('Ctrl Pts',(9.47327458459393,1.42740150969491,3.77254822757006));
#7555=CARTESIAN_POINT('Ctrl Pts',(9.37740190277446,2.85063160470144,2.51502460240537));
#7556=CARTESIAN_POINT('Ctrl Pts',(9.32945963346002,3.26698177317708,1.72772991200983));
#7557=CARTESIAN_POINT('Ctrl Pts',(9.62390099291383,-3.05721247713093,1.61679428011383));
#7558=CARTESIAN_POINT('Ctrl Pts',(9.57595872359942,-2.66759569372247,2.35353764685611));
#7559=CARTESIAN_POINT('Ctrl Pts',(9.48008604177992,-1.33574963323748,3.53031706714705));
#7560=CARTESIAN_POINT('Ctrl Pts',(9.33627109064602,1.33574963323749,3.53031706714703));
#7561=CARTESIAN_POINT('Ctrl Pts',(9.24039840882654,2.66759569372248,2.3535376468561));
#7562=CARTESIAN_POINT('Ctrl Pts',(9.19245613951212,3.05721247713093,1.61679428011382));
#7563=CARTESIAN_POINT('Ctrl Pts',(9.48689749896593,-2.84744318108477,1.5058586482178));
#7564=CARTESIAN_POINT('Ctrl Pts',(9.43895522965151,-2.4845597827435,2.19205069130684));
#7565=CARTESIAN_POINT('Ctrl Pts',(9.34308254783202,-1.24409775678003,3.28808590672403));
#7566=CARTESIAN_POINT('Ctrl Pts',(9.19926759669813,1.24409775678006,3.28808590672402));
#7567=CARTESIAN_POINT('Ctrl Pts',(9.10339491487864,2.48455978274351,2.19205069130682));
#7568=CARTESIAN_POINT('Ctrl Pts',(9.05545264556422,2.84744318108478,1.50585864821778));
#7569=CARTESIAN_POINT('Ctrl Pts',(11.1479080792332,-3.47675197885198,1.8386638238398));
#7570=CARTESIAN_POINT('Ctrl Pts',(11.0999657771109,-3.03366856198811,2.67651064606967));
#7571=CARTESIAN_POINT('Ctrl Pts',(11.0040930624836,-1.51901497956362,4.01476313548051));
#7572=CARTESIAN_POINT('Ctrl Pts',(10.860278045734,1.51901497956361,4.01476313548052));
#7573=CARTESIAN_POINT('Ctrl Pts',(10.7644053311067,3.0336685619881,2.67651064606967));
#7574=CARTESIAN_POINT('Ctrl Pts',(10.7164630289844,3.47675197885198,1.83866382383981));
#7575=CARTESIAN_POINT('Ctrl Pts',(11.01090733667,-3.26698684063499,1.72773052359626));
#7576=CARTESIAN_POINT('Ctrl Pts',(10.9629650345478,-2.85063626371641,2.51502698861378));
#7577=CARTESIAN_POINT('Ctrl Pts',(10.8670923199204,-1.42736726092277,3.77253782025955));
#7578=CARTESIAN_POINT('Ctrl Pts',(10.7232773031708,1.42736726092277,3.77253782025955));
#7579=CARTESIAN_POINT('Ctrl Pts',(10.6274045885434,2.85063626371641,2.51502698861378));
#7580=CARTESIAN_POINT('Ctrl Pts',(10.5794622864212,3.26698684063499,1.72773052359626));
#7581=CARTESIAN_POINT('Ctrl Pts',(10.8739065941069,-3.057221702418,1.61679722335272));
#7582=CARTESIAN_POINT('Ctrl Pts',(10.8259642919846,-2.6676039654447,2.35354333115788));
#7583=CARTESIAN_POINT('Ctrl Pts',(10.7300915773573,-1.33571954228192,3.53031250503859));
#7584=CARTESIAN_POINT('Ctrl Pts',(10.5862765606076,1.33571954228193,3.53031250503859));
#7585=CARTESIAN_POINT('Ctrl Pts',(10.4904038459803,2.66760396544471,2.35354333115788));
#7586=CARTESIAN_POINT('Ctrl Pts',(10.442461543858,3.05722170241801,1.61679722335272));
#7587=CARTESIAN_POINT('Ctrl Pts',(10.7369058515438,-2.84745656420101,1.50586392310919));
#7588=CARTESIAN_POINT('Ctrl Pts',(10.6889635494215,-2.484571667173,2.192059673702));
#7589=CARTESIAN_POINT('Ctrl Pts',(10.5930908347941,-1.24407182364107,3.28808718981763));
#7590=CARTESIAN_POINT('Ctrl Pts',(10.4492758180446,1.24407182364108,3.28808718981762));
#7591=CARTESIAN_POINT('Ctrl Pts',(10.3534031034172,2.48457166717301,2.19205967370197));
#7592=CARTESIAN_POINT('Ctrl Pts',(10.305460801295,2.84745656420102,1.50586392310916));
#7593=CARTESIAN_POINT('Origin',(11.0238490761438,-0.429849779945933,0.997913274973232));
#7594=CARTESIAN_POINT('Ctrl Pts',(11.1020448718976,-1.95024171098983,-2.73386013557053));
#7595=CARTESIAN_POINT('Ctrl Pts',(11.0712404028977,-2.37355302340116,-2.43188441726037));
#7596=CARTESIAN_POINT('Ctrl Pts',(11.0404359338978,-2.72516811805232,-2.03009223981615));
#7597=CARTESIAN_POINT('Ctrl Pts',(11.0096314648979,-2.96834053891712,-1.57047394666944));
#7598=CARTESIAN_POINT('Ctrl Pts',(11.0759796066463,-1.92402331790621,-2.69710704016389));
#7599=CARTESIAN_POINT('Ctrl Pts',(11.0451751376464,-2.34164377552606,-2.3991909817614));
#7600=CARTESIAN_POINT('Ctrl Pts',(11.0143706686465,-2.68853187520334,-2.00280036310181));
#7601=CARTESIAN_POINT('Ctrl Pts',(10.9835661996466,-2.9284351678973,-1.54936102357415));
#7602=CARTESIAN_POINT('Ctrl Pts',(11.049914341395,-1.8978049248226,-2.66035394475725));
#7603=CARTESIAN_POINT('Ctrl Pts',(11.0191098723951,-2.30973452765096,-2.36649754626242));
#7604=CARTESIAN_POINT('Ctrl Pts',(10.9883054033952,-2.65189563235436,-1.97550848638747));
#7605=CARTESIAN_POINT('Ctrl Pts',(10.9575009343953,-2.88852979687749,-1.52824810047886));
#7606=CARTESIAN_POINT('Ctrl Pts',(11.0238490761438,-1.87158653173898,-2.62360084935061));
#7607=CARTESIAN_POINT('Ctrl Pts',(10.9930446071439,-2.27782527977586,-2.33380411076345));
#7608=CARTESIAN_POINT('Ctrl Pts',(10.962240138144,-2.61525938950538,-1.94821660967313));
#7609=CARTESIAN_POINT('Ctrl Pts',(10.9314356691441,-2.84862442585768,-1.50713517738357));
#7610=CARTESIAN_POINT('Ctrl Pts',(11.0238490761438,-2.84858683313225,-1.77828791130292));
#7611=CARTESIAN_POINT('Ctrl Pts',(11.0238490761438,-2.71494761674313,-1.950099643838));
#7612=CARTESIAN_POINT('Ctrl Pts',(11.0238490760976,-2.56437727492177,-2.10888684210166));
#7613=CARTESIAN_POINT('Ctrl Pts',(11.0238490760976,-2.23653062661935,-2.39254456366359));
#7614=CARTESIAN_POINT('Ctrl Pts',(11.0238490761438,-2.05954305124027,-2.51769365192168));
#7615=CARTESIAN_POINT('Ctrl Pts',(11.0238490761438,-1.87158653173898,-2.62360084935061));
#7616=CARTESIAN_POINT('Origin',(11.0238490761438,0.,0.));
#7617=CARTESIAN_POINT('',(12.0768490761438,5.,-6.12323399573677E-16));
#7618=CARTESIAN_POINT('Origin',(12.0768490761438,0.,0.));
#7619=CARTESIAN_POINT('',(11.0238490761438,5.,-6.12323399573677E-16));
#7620=CARTESIAN_POINT('',(11.0238490761438,5.,6.12323399573677E-16));
#7621=CARTESIAN_POINT('Origin',(11.0238490761438,0.,0.));
#7622=CARTESIAN_POINT('Origin',(11.0238490761438,0.,0.));
#7623=CARTESIAN_POINT('Origin',(12.0768490761438,0.,0.));
#7624=CARTESIAN_POINT('',(0.,0.,0.));
#7625=CARTESIAN_POINT('Origin',(24.2263990006525,0.,0.));
#7626=CARTESIAN_POINT('',(24.5263990006525,-7.47952522416948E-16,6.1074958342087));
#7627=CARTESIAN_POINT('Origin',(24.5263990006525,0.,0.));
#7628=CARTESIAN_POINT('',(24.2263103178667,-7.84691924786135E-16,6.40749582110097));
#7629=CARTESIAN_POINT('Origin',(24.2263990006525,-7.47952522416948E-16,
6.1074958342087));
#7630=CARTESIAN_POINT('Origin',(24.2263103178667,-7.84691924786135E-16,
0.));
#7631=CARTESIAN_POINT('Origin',(23.6497386319918,0.,0.));
#7632=CARTESIAN_POINT('',(23.0729895805454,-7.84650172616918E-16,6.40715488876647));
#7633=CARTESIAN_POINT('',(23.6497386319918,-7.84671051911994E-16,6.40732538114918));
#7634=CARTESIAN_POINT('Origin',(23.0729895805454,-7.84650172616918E-16,
0.));
#7635=CARTESIAN_POINT('Origin',(24.5263990006525,0.,0.));
#7636=CARTESIAN_POINT('Origin',(23.0730782633312,0.,0.));
#7637=CARTESIAN_POINT('',(22.7730782633312,-7.47910770247731E-16,6.1071549018742));
#7638=CARTESIAN_POINT('Origin',(23.0730782633312,-7.47910770247731E-16,
6.1071549018742));
#7639=CARTESIAN_POINT('Origin',(22.7730782633312,0.,0.));
#7640=CARTESIAN_POINT('Origin',(22.7730782633312,0.,-6.40706623219228));
#7641=CARTESIAN_POINT('',(0.,0.,0.));
#7642=CARTESIAN_POINT('Origin',(80.1322559480305,0.,0.));
#7643=CARTESIAN_POINT('',(83.3472004496623,-2.62083096187227,2.64334895679097));
#7644=CARTESIAN_POINT('',(83.0989050616807,-2.62063375225138,2.64301435574924));
#7645=CARTESIAN_POINT('',(80.1322559480305,-2.62112000711956,2.64359555733806));
#7646=CARTESIAN_POINT('',(82.4430344427077,-2.13746972315899,-3.04920351925858));
#7647=CARTESIAN_POINT('Ctrl Pts',(82.4430344427077,-2.13746972315899,-3.04920351925858));
#7648=CARTESIAN_POINT('Ctrl Pts',(82.448599020418,-2.05742239043371,-3.10508886440805));
#7649=CARTESIAN_POINT('Ctrl Pts',(82.4542421068107,-1.97502380466239,-3.15787593603748));
#7650=CARTESIAN_POINT('Ctrl Pts',(82.4599027186458,-1.8905590270017,-3.20738255279828));
#7651=CARTESIAN_POINT('Ctrl Pts',(82.4661987179127,-1.79661332047366,-3.26244614519996));
#7652=CARTESIAN_POINT('Ctrl Pts',(82.4725160793993,-1.70011081204737,-3.31345191940099));
#7653=CARTESIAN_POINT('Ctrl Pts',(82.4787882071852,-1.60145546459568,-3.36018801727306));
#7654=CARTESIAN_POINT('Ctrl Pts',(82.4851385165621,-1.50157038581804,-3.40750667701421));
#7655=CARTESIAN_POINT('Ctrl Pts',(82.4914422189564,-1.39947851936814,-3.45044862674078));
#7656=CARTESIAN_POINT('Ctrl Pts',(82.4976522109053,-1.29561251865481,-3.4888308753646));
#7657=CARTESIAN_POINT('Ctrl Pts',(82.5037761074298,-1.19318651778106,-3.52668099190014));
#7658=CARTESIAN_POINT('Ctrl Pts',(82.5098088434891,-1.08903531916436,-3.56009707952411));
#7659=CARTESIAN_POINT('Ctrl Pts',(82.5157283399517,-0.983585676573463,-3.58893767538103));
#7660=CARTESIAN_POINT('Ctrl Pts',(82.5216461639355,-0.878165827446473,-3.61777012269206));
#7661=CARTESIAN_POINT('Ctrl Pts',(82.5274508110353,-0.771448321683715,-3.64202961671188));
#7662=CARTESIAN_POINT('Ctrl Pts',(82.5331437584232,-0.663870498101131,-3.66160866851016));
#7663=CARTESIAN_POINT('Ctrl Pts',(82.5388366319855,-0.556294069576837,-3.68118746640929));
#7664=CARTESIAN_POINT('Ctrl Pts',(82.5444178817885,-0.447857403542125,-3.69608582043075));
#7665=CARTESIAN_POINT('Ctrl Pts',(82.5499119917177,-0.339007936737362,-3.70623138116809));
#7666=CARTESIAN_POINT('Ctrl Pts',(82.5555437320619,-0.227431732122251,-3.71663109367008));
#7667=CARTESIAN_POINT('Ctrl Pts',(82.561083992165,-0.115421821891503,-3.72203652187028));
#7668=CARTESIAN_POINT('Ctrl Pts',(82.5665823292253,-0.00347010483924686,
-3.72241073611585));
#7669=CARTESIAN_POINT('Ctrl Pts',(82.5719534018203,0.105890378672952,-3.72277628880151));
#7670=CARTESIAN_POINT('Ctrl Pts',(82.5772848247073,0.215195189456353,-3.71834069411313));
#7671=CARTESIAN_POINT('Ctrl Pts',(82.5826411259721,0.323977809003443,-3.70911160173114));
#7672=CARTESIAN_POINT('Ctrl Pts',(82.5878495140364,0.429756418016825,-3.70013736891079));
#7673=CARTESIAN_POINT('Ctrl Pts',(82.5930817674659,0.535041662344979,-3.68663025460312));
#7674=CARTESIAN_POINT('Ctrl Pts',(82.5984092695587,0.639397738760414,-3.66864062923815));
#7675=CARTESIAN_POINT('Ctrl Pts',(82.5987552909183,0.64617566785591,-3.66747220273759));
#7676=CARTESIAN_POINT('Ctrl Pts',(82.5991017140848,0.652949694448339,-3.66628487290753));
#7677=CARTESIAN_POINT('Ctrl Pts',(82.5994485586168,0.659719706360457,-3.6650786559658));
#7678=CARTESIAN_POINT('Ctrl Pts',(82.6044019668751,0.756404617975652,-3.64785224928972));
#7679=CARTESIAN_POINT('Ctrl Pts',(82.6094418421539,0.85226762557606,-3.62677244801423));
#7680=CARTESIAN_POINT('Ctrl Pts',(82.6146291074746,0.946957722867219,-3.60191904664229));
#7681=CARTESIAN_POINT('Ctrl Pts',(82.6153947659428,0.960934311757064,-3.59825059784535));
#7682=CARTESIAN_POINT('Ctrl Pts',(82.616163635567,0.974885430209022,-3.59449997452717));
#7683=CARTESIAN_POINT('Ctrl Pts',(82.6169359122638,0.988810037286412,-3.59066747321032));
#7684=CARTESIAN_POINT('Ctrl Pts',(82.6169385232966,0.98885711575661,-3.59065451569575));
#7685=CARTESIAN_POINT('Ctrl Pts',(82.6169411343683,0.988904193923786,-3.59064155724526));
#7686=CARTESIAN_POINT('Ctrl Pts',(82.616943745479,0.988951271787904,-3.59062859785889));
#7687=CARTESIAN_POINT('Ctrl Pts',(82.6223437588327,1.08631255847876,-3.56382741315182));
#7688=CARTESIAN_POINT('Ctrl Pts',(82.6279228623114,1.18268025289156,-3.53292971855098));
#7689=CARTESIAN_POINT('Ctrl Pts',(82.6336067866526,1.27770342316418,-3.49806263639509));
#7690=CARTESIAN_POINT('Ctrl Pts',(82.634189838298,1.28745081113927,-3.49448600370269));
#7691=CARTESIAN_POINT('Ctrl Pts',(82.6347739929172,1.29718402569802,-3.49086764046184));
#7692=CARTESIAN_POINT('Ctrl Pts',(82.6353591703451,1.30690267098624,-3.48720770968247));
#7693=CARTESIAN_POINT('Ctrl Pts',(82.641641165732,1.41123424967816,-3.44791762914239));
#7694=CARTESIAN_POINT('Ctrl Pts',(82.6480404752863,1.51389054851696,-3.4038324220682));
#7695=CARTESIAN_POINT('Ctrl Pts',(82.6544691591425,1.61443137085044,-3.35516312012428));
#7696=CARTESIAN_POINT('Ctrl Pts',(82.6608915579549,1.71487389880572,-3.30654140003479));
#7697=CARTESIAN_POINT('Ctrl Pts',(82.6673429189712,1.81320529683611,-3.25334486330551));
#7698=CARTESIAN_POINT('Ctrl Pts',(82.673753583758,1.90901390837151,-3.19581575437501));
#7699=CARTESIAN_POINT('Ctrl Pts',(82.6801598752994,2.0047571609184,-3.13832589081409));
#7700=CARTESIAN_POINT('Ctrl Pts',(82.6865253269448,2.09798121640403,-3.07650952231491));
#7701=CARTESIAN_POINT('Ctrl Pts',(82.6928025349669,2.18829974073378,-3.01063669396523));
#7702=CARTESIAN_POINT('Ctrl Pts',(82.6990774796109,2.27858569883874,-2.94478761743559));
#7703=CARTESIAN_POINT('Ctrl Pts',(82.7052641575682,2.36596828259258,-2.87488506236255));
#7704=CARTESIAN_POINT('Ctrl Pts',(82.7113394306864,2.45008446654331,-2.80122550716461));
#7705=CARTESIAN_POINT('Ctrl Pts',(82.7174139832278,2.53419067363046,-2.72757468858904));
#7706=CARTESIAN_POINT('Ctrl Pts',(82.7233771574382,2.61503123368847,-2.6501677521564));
#7707=CARTESIAN_POINT('Ctrl Pts',(82.7292306714799,2.69226584882458,-2.56932746171694));
#7708=CARTESIAN_POINT('Ctrl Pts',(82.735084907537,2.76950999064356,-2.48847719984422));
#7709=CARTESIAN_POINT('Ctrl Pts',(82.740829536682,2.84314719537528,-2.40419267740033));
#7710=CARTESIAN_POINT('Ctrl Pts',(82.7464905348952,2.91286057875016,-2.31682369884723));
#7711=CARTESIAN_POINT('Ctrl Pts',(82.7521570798643,2.98264226865268,-2.22936911447127));
#7712=CARTESIAN_POINT('Ctrl Pts',(82.7577400007629,3.04849224778961,-2.13882391940644));
#7713=CARTESIAN_POINT('Ctrl Pts',(82.7632877940693,3.11011851311843,-2.04556718326659));
#7714=CARTESIAN_POINT('Ctrl Pts',(82.7688382903374,3.17177480361737,-1.9522650111531));
#7715=CARTESIAN_POINT('Ctrl Pts',(82.7743539191269,3.22920295013996,-1.85624852227942));
#7716=CARTESIAN_POINT('Ctrl Pts',(82.7799022412833,3.28214013584634,-1.75792741509752));
#7717=CARTESIAN_POINT('Ctrl Pts',(82.7854593714353,3.3351613596614,-1.6594502225518));
#7718=CARTESIAN_POINT('Ctrl Pts',(82.7910497493793,3.38367687065512,-1.55866097056305));
#7719=CARTESIAN_POINT('Ctrl Pts',(82.7967547537525,3.42745823752841,-1.45600343909067));
#7720=CARTESIAN_POINT('Ctrl Pts',(82.8020073577273,3.46776779149483,-1.36148653383001));
#7721=CARTESIAN_POINT('Ctrl Pts',(82.8073576638974,3.50406423704884,-1.26538626329073));
#7722=CARTESIAN_POINT('Ctrl Pts',(82.812873362228,3.53620220344326,-1.16807374112353));
#7723=CARTESIAN_POINT('Ctrl Pts',(82.8128756709941,3.53621565578332,-1.16803300795691));
#7724=CARTESIAN_POINT('Ctrl Pts',(82.8128779797893,3.53622910739548,-1.16799227457744));
#7725=CARTESIAN_POINT('Ctrl Pts',(82.8128802886134,3.53624255827976,-1.16795154098513));
#7726=CARTESIAN_POINT('Ctrl Pts',(82.8183364857455,3.56802959447665,-1.07169019891507));
#7727=CARTESIAN_POINT('Ctrl Pts',(82.8239655492868,3.59583022943719,-0.973972859449433));
#7728=CARTESIAN_POINT('Ctrl Pts',(82.8296926587345,3.61955415052866,-0.875165751197072));
#7729=CARTESIAN_POINT('Ctrl Pts',(82.8302450796905,3.62184249359063,-0.86563509394313));
#7730=CARTESIAN_POINT('Ctrl Pts',(82.8307984128648,3.62409292118861,-0.856094334891532));
#7731=CARTESIAN_POINT('Ctrl Pts',(82.8313525911108,3.62630536186244,-0.846543826418543));
#7732=CARTESIAN_POINT('Ctrl Pts',(82.8376442504153,3.65142349497653,-0.738115633984115));
#7733=CARTESIAN_POINT('Ctrl Pts',(82.8440442952487,3.67164363836166,-0.628425160901477));
#7734=CARTESIAN_POINT('Ctrl Pts',(82.8504661980963,3.68689646460076,-0.517952854476233));
#7735=CARTESIAN_POINT('Ctrl Pts',(82.8568818350485,3.70213440855105,-0.407588336649791));
#7736=CARTESIAN_POINT('Ctrl Pts',(82.8633189471795,3.71241508912789,-0.296443513022478));
#7737=CARTESIAN_POINT('Ctrl Pts',(82.869709517214,3.71771058909135,-0.184992936878773));
#7738=CARTESIAN_POINT('Ctrl Pts',(82.876095800766,3.72300253709186,-0.0736171163425392));
#7739=CARTESIAN_POINT('Ctrl Pts',(82.8824354149202,3.72331619094564,0.0380640758994348));
#7740=CARTESIAN_POINT('Ctrl Pts',(82.8886826470533,3.71866065339773,0.149581257438668));
#7741=CARTESIAN_POINT('Ctrl Pts',(82.8949276751545,3.71400675832982,0.261059095564304));
#7742=CARTESIAN_POINT('Ctrl Pts',(82.9010803057731,3.70438725083538,0.372373051082597));
#7743=CARTESIAN_POINT('Ctrl Pts',(82.9071190301882,3.68984615519603,0.483058114605687));
#7744=CARTESIAN_POINT('Ctrl Pts',(82.9131571001419,3.67530663548319,0.593731182366596));
#7745=CARTESIAN_POINT('Ctrl Pts',(82.9190812929002,3.65584656994163,0.703775474025912));
#7746=CARTESIAN_POINT('Ctrl Pts',(82.9248948207163,3.63154455459684,0.81273006150251));
#7747=CARTESIAN_POINT('Ctrl Pts',(82.9307091394138,3.60723923316746,0.921699471333437));
#7748=CARTESIAN_POINT('Ctrl Pts',(82.9364128470765,3.57809053510775,1.02957882216876));
#7749=CARTESIAN_POINT('Ctrl Pts',(82.9420332222564,3.54421269521027,1.13591151444198));
#7750=CARTESIAN_POINT('Ctrl Pts',(82.9476592811328,3.51030059579144,1.2423517373946));
#7751=CARTESIAN_POINT('Ctrl Pts',(82.9532020137706,3.47164958467528,1.34724206263577));
#7752=CARTESIAN_POINT('Ctrl Pts',(82.9587109769047,3.42841224504195,1.45013026888811));
#7753=CARTESIAN_POINT('Ctrl Pts',(82.9642227061628,3.38515319536202,1.5530701366851));
#7754=CARTESIAN_POINT('Ctrl Pts',(82.9697009311859,3.33730292490927,1.6540056815073));
#7755=CARTESIAN_POINT('Ctrl Pts',(82.9752139615805,3.28505590947795,1.75249199067341));
#7756=CARTESIAN_POINT('Ctrl Pts',(82.9807359802808,3.23272371183045,1.85113886943394));
#7757=CARTESIAN_POINT('Ctrl Pts',(82.9862933738097,3.1759800559052,1.94732817734345));
#7758=CARTESIAN_POINT('Ctrl Pts',(82.9919678899615,3.11506709186677,2.04062478348433));
#7759=CARTESIAN_POINT('Ctrl Pts',(82.9972893737137,3.05794374605924,2.12811706660311));
#7760=CARTESIAN_POINT('Ctrl Pts',(83.0027144147527,2.99715390579646,2.21306510187555));
#7761=CARTESIAN_POINT('Ctrl Pts',(83.0083144719426,2.93293887122742,2.29512480585364));
#7762=CARTESIAN_POINT('Ctrl Pts',(83.0083169090159,2.93291092566555,2.29516051718743));
#7763=CARTESIAN_POINT('Ctrl Pts',(83.0083193461223,2.93288297945502,2.29519622797522));
#7764=CARTESIAN_POINT('Ctrl Pts',(83.0083217832619,2.93285503259586,2.29523193821698));
#7765=CARTESIAN_POINT('Ctrl Pts',(83.013748510229,2.87062635440728,2.3747471757048));
#7766=CARTESIAN_POINT('Ctrl Pts',(83.019350976778,2.80499626954421,2.45177672341973));
#7767=CARTESIAN_POINT('Ctrl Pts',(83.0250542593079,2.73621649003507,2.52604381205996));
#7768=CARTESIAN_POINT('Ctrl Pts',(83.0256152719976,2.72945085482468,2.53334921538436));
#7769=CARTESIAN_POINT('Ctrl Pts',(83.0261772601821,2.72265478377114,2.54062787998606));
#7770=CARTESIAN_POINT('Ctrl Pts',(83.0267401525496,2.71582854307071,2.54787953697994));
#7771=CARTESIAN_POINT('Ctrl Pts',(83.0330173539257,2.6397044205996,2.62874777022077));
#7772=CARTESIAN_POINT('Ctrl Pts',(83.0394064576322,2.5598227077811,2.70625903217862));
#7773=CARTESIAN_POINT('Ctrl Pts',(83.045820175139,2.47654279495297,2.78008926792871));
#7774=CARTESIAN_POINT('Ctrl Pts',(83.052227397231,2.39334722284971,2.85384473300015));
#7775=CARTESIAN_POINT('Ctrl Pts',(83.0586588407085,2.30676053662994,2.92392692670572));
#7776=CARTESIAN_POINT('Ctrl Pts',(83.0650456575877,2.21716027063657,2.99004955358705));
#7777=CARTESIAN_POINT('Ctrl Pts',(83.0714278944391,2.12762425757619,3.05612476350296));
#7778=CARTESIAN_POINT('Ctrl Pts',(83.0777653772024,2.03507907421888,3.11824626719335));
#7779=CARTESIAN_POINT('Ctrl Pts',(83.0840115212539,1.93991852507007,3.17616147120232));
#7780=CARTESIAN_POINT('Ctrl Pts',(83.0902552902423,1.84479416021438,3.23405465326274));
#7781=CARTESIAN_POINT('Ctrl Pts',(83.0964077076695,1.74705645069182,3.28774480190484));
#7782=CARTESIAN_POINT('Ctrl Pts',(83.1024463695484,1.64711496019518,3.33701081475946));
#7783=CARTESIAN_POINT('Ctrl Pts',(83.1084842289857,1.54718675032443,3.3862702809488));
#7784=CARTESIAN_POINT('Ctrl Pts',(83.1144083654278,1.44505535153882,3.43110675608568));
#7785=CARTESIAN_POINT('Ctrl Pts',(83.1202210958824,1.34114609734128,3.47133016523115));
#7786=CARTESIAN_POINT('Ctrl Pts',(83.1260344917427,1.23722494824878,3.51155817890613));
#7787=CARTESIAN_POINT('Ctrl Pts',(83.1317365372578,1.13152552810977,3.54717194893531));
#7788=CARTESIAN_POINT('Ctrl Pts',(83.1373536485256,1.0244892779953,3.57801342989723));
#7789=CARTESIAN_POINT('Ctrl Pts',(83.1429763325976,0.917346835920189,3.60888550906611));
#7790=CARTESIAN_POINT('Ctrl Pts',(83.1485140843379,0.808864893437081,3.63497560174989));
#7791=CARTESIAN_POINT('Ctrl Pts',(83.1540156802369,0.699502403811492,3.65615992849922));
#7792=CARTESIAN_POINT('Ctrl Pts',(83.1595199628709,0.590086506405814,3.67735460073235));
#7793=CARTESIAN_POINT('Ctrl Pts',(83.1649883472167,0.479789205696713,3.69363837602126));
#7794=CARTESIAN_POINT('Ctrl Pts',(83.1704885251433,0.369086461722915,3.70492623568189));
#7795=CARTESIAN_POINT('Ctrl Pts',(83.1759976774181,0.258203089962481,3.7162325131435));
#7796=CARTESIAN_POINT('Ctrl Pts',(83.181539174532,0.146913031264152,3.72252607292026));
#7797=CARTESIAN_POINT('Ctrl Pts',(83.1871944214616,0.0357104127877853,3.72376672713407));
#7798=CARTESIAN_POINT('Ctrl Pts',(83.1922556540262,-0.0638117337991707,
3.72487706583133));
#7799=CARTESIAN_POINT('Ctrl Pts',(83.1974084980998,-0.163264124747811,3.72194044402702));
#7800=CARTESIAN_POINT('Ctrl Pts',(83.2027150991779,-0.262281572855464,3.71496438230409));
#7801=CARTESIAN_POINT('Ctrl Pts',(83.2031054575553,-0.269565385942157,3.7144512168909));
#7802=CARTESIAN_POINT('Ctrl Pts',(83.2034966479436,-0.27684686462192,3.71391620668298));
#7803=CARTESIAN_POINT('Ctrl Pts',(83.2038886950801,-0.284125872785762,3.71335936092993));
#7804=CARTESIAN_POINT('Ctrl Pts',(83.203891136264,-0.284171197431151,3.71335589358442));
#7805=CARTESIAN_POINT('Ctrl Pts',(83.2038935774811,-0.284216521980756,3.71335242539229));
#7806=CARTESIAN_POINT('Ctrl Pts',(83.2038960187314,-0.284261846434547,3.71334895635357));
#7807=CARTESIAN_POINT('Ctrl Pts',(83.2093252565624,-0.38506152120613,3.70563396047512));
#7808=CARTESIAN_POINT('Ctrl Pts',(83.2149301683938,-0.485673358945827,3.69370039164411));
#7809=CARTESIAN_POINT('Ctrl Pts',(83.2206360185141,-0.585726878726986,3.67760519262689));
#7810=CARTESIAN_POINT('Ctrl Pts',(83.2211983295403,-0.595587144278816,3.676019012183));
#7811=CARTESIAN_POINT('Ctrl Pts',(83.2217616208878,-0.605441957224624,3.67439244250633));
#7812=CARTESIAN_POINT('Ctrl Pts',(83.2223258210251,-0.615290943611994,3.6727255573895));
#7813=CARTESIAN_POINT('Ctrl Pts',(83.2286076879843,-0.724950651362645,3.65416627346153));
#7814=CARTESIAN_POINT('Ctrl Pts',(83.2350016713654,-0.833892609821066,3.63060534416091));
#7815=CARTESIAN_POINT('Ctrl Pts',(83.2414205881829,-0.941646888095381,3.60216349040293));
#7816=CARTESIAN_POINT('Ctrl Pts',(83.2478335756957,-1.04930163120416,3.57374790905536));
#7817=CARTESIAN_POINT('Ctrl Pts',(83.2542711057617,-1.15577102706027,3.54046075836396));
#7818=CARTESIAN_POINT('Ctrl Pts',(83.2606643943902,-1.26060657552585,3.50245879728538));
#7819=CARTESIAN_POINT('Ctrl Pts',(83.267053345539,-1.36537099908479,3.46448261835774));
#7820=CARTESIAN_POINT('Ctrl Pts',(83.2733979224415,-1.46850389809735,3.42179820146728));
#7821=CARTESIAN_POINT('Ctrl Pts',(83.2796516060403,-1.56957589780418,3.37459449492827));
#7822=CARTESIAN_POINT('Ctrl Pts',(83.2859035825247,-1.67062030713583,3.32740367393597));
#7823=CARTESIAN_POINT('Ctrl Pts',(83.292064632062,-1.76960498350736,3.27569609467376));
#7824=CARTESIAN_POINT('Ctrl Pts',(83.2981124330876,-1.86611799349614,3.21969128823285));
#7825=CARTESIAN_POINT('Ctrl Pts',(83.3041590631163,-1.96261231629155,3.16369732564241));
#7826=CARTESIAN_POINT('Ctrl Pts',(83.3100924911403,-2.05663590320112,3.10340778724449));
#7827=CARTESIAN_POINT('Ctrl Pts',(83.3159151518672,-2.14779403729,3.03907244084058));
#7828=CARTESIAN_POINT('Ctrl Pts',(83.3217404122008,-2.238992870176,2.97470837104039));
#7829=CARTESIAN_POINT('Ctrl Pts',(83.327454886879,-2.32732359545313,2.90629480158804));
#7830=CARTESIAN_POINT('Ctrl Pts',(83.3330851650687,-2.41240887718516,2.83411292117315));
#7831=CARTESIAN_POINT('Ctrl Pts',(83.3378403569136,-2.48426977360557,2.77314991410147));
#7832=CARTESIAN_POINT('Ctrl Pts',(83.3425359671718,-2.55381591599853,2.7094994265022));
#7833=CARTESIAN_POINT('Ctrl Pts',(83.3472004496623,-2.62083096187227,2.64334895679097));
#7834=CARTESIAN_POINT('',(82.4430005297901,2.16151778945158,-3.03095833168065));
#7835=CARTESIAN_POINT('Origin',(82.4430005297901,0.,0.));
#7836=CARTESIAN_POINT('Ctrl Pts',(82.4430005297901,2.16151778945158,-3.03095833168064));
#7837=CARTESIAN_POINT('Ctrl Pts',(82.4497525870341,2.2643871255196,-2.95759740897315));
#7838=CARTESIAN_POINT('Ctrl Pts',(82.4564309935575,2.36343920336681,-2.8790005193258));
#7839=CARTESIAN_POINT('Ctrl Pts',(82.463090623901,2.45821022550934,-2.79559583490443));
#7840=CARTESIAN_POINT('Ctrl Pts',(82.4697568618797,2.55307527874839,-2.71210839698148));
#7841=CARTESIAN_POINT('Ctrl Pts',(82.4764047311352,2.64365116871439,-2.62380392905304));
#7842=CARTESIAN_POINT('Ctrl Pts',(82.4830735939787,2.72951313809316,-2.53113618409738));
#7843=CARTESIAN_POINT('Ctrl Pts',(82.4897405696392,2.81535080988868,-2.43849466265212));
#7844=CARTESIAN_POINT('Ctrl Pts',(82.4964287755875,2.89647757511398,-2.34149239606588));
#7845=CARTESIAN_POINT('Ctrl Pts',(82.5031567095667,2.97250377452681,-2.24060427989571));
#7846=CARTESIAN_POINT('Ctrl Pts',(82.5098729756242,3.04839812547926,-2.13989112897292));
#7847=CARTESIAN_POINT('Ctrl Pts',(82.5166289021824,3.11920981016223,-2.03530546536337));
#7848=CARTESIAN_POINT('Ctrl Pts',(82.5234197668534,3.18458147885758,-1.9273417200709));
#7849=CARTESIAN_POINT('Ctrl Pts',(82.5290415570546,3.23869915375146,-1.83796436464048));
#7850=CARTESIAN_POINT('Ctrl Pts',(82.5346868339601,3.28908916023992,-1.74627221537606));
#7851=CARTESIAN_POINT('Ctrl Pts',(82.5403409406944,3.33556346134786,-1.65255871416402));
#7852=CARTESIAN_POINT('Ctrl Pts',(82.5403413804331,3.33556707580869,-1.65255142575362));
#7853=CARTESIAN_POINT('Ctrl Pts',(82.5403418201718,3.33557069024584,-1.65254413733098));
#7854=CARTESIAN_POINT('Ctrl Pts',(82.5403422599106,3.33557430465931,-1.65253684889611));
#7855=CARTESIAN_POINT('Ctrl Pts',(82.5464419928859,3.38571079068679,-1.55143703950375));
#7856=CARTESIAN_POINT('Ctrl Pts',(82.5525511172057,3.43126617851106,-1.44802709255062));
#7857=CARTESIAN_POINT('Ctrl Pts',(82.5586922252033,3.47204912375138,-1.34275980756767));
#7858=CARTESIAN_POINT('Ctrl Pts',(82.5648327804175,3.51282839797113,-1.23750199807418));
#7859=CARTESIAN_POINT('Ctrl Pts',(82.5710053901627,3.54883620716724,-1.13038720018602));
#7860=CARTESIAN_POINT('Ctrl Pts',(82.5772071341509,3.57991676752814,-1.02187841964011));
#7861=CARTESIAN_POINT('Ctrl Pts',(82.583411964925,3.61101279757595,-0.913315631159872));
#7862=CARTESIAN_POINT('Ctrl Pts',(82.5896459347367,3.63717667625632,-0.803357419154788));
#7863=CARTESIAN_POINT('Ctrl Pts',(82.5958801874174,3.65828700678163,-0.692478117868246));
#7864=CARTESIAN_POINT('Ctrl Pts',(82.6021161755057,3.6794032137175,-0.581567951489553));
#7865=CARTESIAN_POINT('Ctrl Pts',(82.6083523050562,3.69546292697117,-0.469736079958543));
#7866=CARTESIAN_POINT('Ctrl Pts',(82.6145349776752,3.70638020509523,-0.357469063727132));
#7867=CARTESIAN_POINT('Ctrl Pts',(82.6207234444741,3.71730771450215,-0.245096834860658));
#7868=CARTESIAN_POINT('Ctrl Pts',(82.6268580629749,3.72308283210855,-0.132288527659337));
#7869=CARTESIAN_POINT('Ctrl Pts',(82.6328635227856,3.72365829592863,-0.0195456358231097));
#7870=CARTESIAN_POINT('Ctrl Pts',(82.63531318067,3.72389303057484,0.0264427684947558));
#7871=CARTESIAN_POINT('Ctrl Pts',(82.6377411248295,3.72326308981242,0.0724201216892056));
#7872=CARTESIAN_POINT('Ctrl Pts',(82.6401414282941,3.72176735365084,0.11835168109134));
#7873=CARTESIAN_POINT('Ctrl Pts',(82.6401428334758,3.72176647801945,0.118378570268839));
#7874=CARTESIAN_POINT('Ctrl Pts',(82.6401442386485,3.72176560209123,0.118405459443261));
#7875=CARTESIAN_POINT('Ctrl Pts',(82.6401456438123,3.72176472586617,0.118432348614587));
#7876=CARTESIAN_POINT('Ctrl Pts',(82.645522635828,3.71841176773665,0.221326307545291));
#7877=CARTESIAN_POINT('Ctrl Pts',(82.6507682282706,3.7107094660618,0.324178372433314));
#7878=CARTESIAN_POINT('Ctrl Pts',(82.6559448084897,3.69870088117316,0.426600109422855));
#7879=CARTESIAN_POINT('Ctrl Pts',(82.6564326859769,3.69756910730466,0.436253057423465));
#7880=CARTESIAN_POINT('Ctrl Pts',(82.6569199504623,3.69639910806877,0.445902154317524));
#7881=CARTESIAN_POINT('Ctrl Pts',(82.6574066541737,3.69519093559596,0.455547057373284));
#7882=CARTESIAN_POINT('Ctrl Pts',(82.6630537803773,3.6811727510821,0.567454946103847));
#7883=CARTESIAN_POINT('Ctrl Pts',(82.6686259946562,3.66201198643677,0.678802678279904));
#7884=CARTESIAN_POINT('Ctrl Pts',(82.6741977677731,3.63781636838717,0.78909978021698));
#7885=CARTESIAN_POINT('Ctrl Pts',(82.6797659318231,3.61363642283602,0.89932543817782));
#7886=CARTESIAN_POINT('Ctrl Pts',(82.6853340641559,3.5844286005684,1.00850181621864));
#7887=CARTESIAN_POINT('Ctrl Pts',(82.6909619773351,3.55034171631595,1.11616037592857));
#7888=CARTESIAN_POINT('Ctrl Pts',(82.6965885352234,3.51626304072669,1.22379300974715));
#7889=CARTESIAN_POINT('Ctrl Pts',(82.702275109538,3.47730796553248,1.32990859917549));
#7890=CARTESIAN_POINT('Ctrl Pts',(82.7080619420672,3.43366074693369,1.43405961383778));
#7891=CARTESIAN_POINT('Ctrl Pts',(82.7138482053755,3.39001782168696,1.53820038370127));
#7892=CARTESIAN_POINT('Ctrl Pts',(82.7197348588063,3.34168387046001,1.64037701333392));
#7893=CARTESIAN_POINT('Ctrl Pts',(82.7257395141122,3.28887486217381,1.74016206022673));
#7894=CARTESIAN_POINT('Ctrl Pts',(82.7317449192916,3.23605925899219,1.83995956847735));
#7895=CARTESIAN_POINT('Ctrl Pts',(82.7378684178647,3.17876757442851,1.93736492912828));
#7896=CARTESIAN_POINT('Ctrl Pts',(82.7441034140718,3.11724548796642,2.0319698863094));
#7897=CARTESIAN_POINT('Ctrl Pts',(82.7503405809174,3.05570198333541,2.12660777906));
#7898=CARTESIAN_POINT('Ctrl Pts',(82.7566893021505,2.98992512603072,2.21844332399032));
#7899=CARTESIAN_POINT('Ctrl Pts',(82.7631184329245,2.92018983143804,2.3070868990241));
#7900=CARTESIAN_POINT('Ctrl Pts',(82.7695555892579,2.85036748545784,2.39584112887401));
#7901=CARTESIAN_POINT('Ctrl Pts',(82.7760732421521,2.77657669642733,2.48139537150511));
#7902=CARTESIAN_POINT('Ctrl Pts',(82.7826165146318,2.69912336244941,2.56337790417287));
#7903=CARTESIAN_POINT('Ctrl Pts',(82.7891640304413,2.62161979977606,2.6454136027336));
#7904=CARTESIAN_POINT('Ctrl Pts',(82.7957369546042,2.54044870904736,2.72387282576453));
#7905=CARTESIAN_POINT('Ctrl Pts',(82.8022593265139,2.45594916272644,2.79840375151851));
#7906=CARTESIAN_POINT('Ctrl Pts',(82.8087929615909,2.37130369824371,2.87306338110769));
#7907=CARTESIAN_POINT('Ctrl Pts',(82.8152754528664,2.28331793548545,2.94378083250582));
#7908=CARTESIAN_POINT('Ctrl Pts',(82.8216143153064,2.19236970908168,3.01022632126189));
#7909=CARTESIAN_POINT('Ctrl Pts',(82.8267383484441,2.11885151392845,3.0639376755409));
#7910=CARTESIAN_POINT('Ctrl Pts',(82.8317680624639,2.04339817135242,3.11485788892921));
#7911=CARTESIAN_POINT('Ctrl Pts',(82.8366503980456,1.96622925062276,3.16282692428072));
#7912=CARTESIAN_POINT('Ctrl Pts',(82.8366527886688,1.96619146505635,3.16285041219728));
#7913=CARTESIAN_POINT('Ctrl Pts',(82.8366551792591,1.96615367902892,3.16287389943928));
#7914=CARTESIAN_POINT('Ctrl Pts',(82.8366575698165,1.9661158925405,3.16289738600667));
#7915=CARTESIAN_POINT('Ctrl Pts',(82.841950133003,1.88245867630496,3.21489536012051));
#7916=CARTESIAN_POINT('Ctrl Pts',(82.8470813568417,1.7965374989223,3.26358628833678));
#7917=CARTESIAN_POINT('Ctrl Pts',(82.8521147636254,1.70866270441033,3.30879236920142));
#7918=CARTESIAN_POINT('Ctrl Pts',(82.8526922604478,1.69858058373519,3.3139789891538));
#7919=CARTESIAN_POINT('Ctrl Pts',(82.8532684696442,1.68847280233983,3.31911974325924));
#7920=CARTESIAN_POINT('Ctrl Pts',(82.8538434871523,1.67833987220444,3.32421436956907));
#7921=CARTESIAN_POINT('Ctrl Pts',(82.8594246728968,1.57998849259643,3.37366339561229));
#7922=CARTESIAN_POINT('Ctrl Pts',(82.864894200596,1.47926182311506,3.41876625740564));
#7923=CARTESIAN_POINT('Ctrl Pts',(82.8703338865973,1.37660580206139,3.45933022664339));
#7924=CARTESIAN_POINT('Ctrl Pts',(82.8757674440819,1.27406543642321,3.49984849527179));
#7925=CARTESIAN_POINT('Ctrl Pts',(82.881171656312,1.1696003477985,3.53583845902318));
#7926=CARTESIAN_POINT('Ctrl Pts',(82.8866144035847,1.06366249754844,3.56715439087171));
#7927=CARTESIAN_POINT('Ctrl Pts',(82.892094624789,0.956995253198249,3.59868593645864));
#7928=CARTESIAN_POINT('Ctrl Pts',(82.8976142242023,0.848835056519796,3.62547909822655));
#7929=CARTESIAN_POINT('Ctrl Pts',(82.9032230550498,0.739647643605751,3.6474276875812));
#7930=CARTESIAN_POINT('Ctrl Pts',(82.9087862130298,0.631349346870345,3.66919754895456));
#7931=CARTESIAN_POINT('Ctrl Pts',(82.9144372918968,0.522040595941809,3.68620165227875));
#7932=CARTESIAN_POINT('Ctrl Pts',(82.9202026482306,0.41217821478049,3.69837446221263));
#7933=CARTESIAN_POINT('Ctrl Pts',(82.9259668521448,0.302337793676463,3.71054483896056));
#7934=CARTESIAN_POINT('Ctrl Pts',(82.9318453637412,0.191944025268312,3.71788595476851));
#7935=CARTESIAN_POINT('Ctrl Pts',(82.9378405423052,0.081454649124195,3.72036809750293));
#7936=CARTESIAN_POINT('Ctrl Pts',(82.9438360708962,-0.0290411779126,3.72285038515659));
#7937=CARTESIAN_POINT('Ctrl Pts',(82.9499482803377,-0.139632588322064,3.72047315281383));
#7938=CARTESIAN_POINT('Ctrl Pts',(82.956154973994,-0.249861298021894,3.71324156078738));
#7939=CARTESIAN_POINT('Ctrl Pts',(82.9624522619302,-0.361698930465173,3.70590441483661));
#7940=CARTESIAN_POINT('Ctrl Pts',(82.968846785684,-0.473163183084761,3.69357000063643));
#7941=CARTESIAN_POINT('Ctrl Pts',(82.9752901691881,-0.583775300960439,3.6762807804806));
#7942=CARTESIAN_POINT('Ctrl Pts',(82.9816499159366,-0.692951645430586,3.65921597879699));
#7943=CARTESIAN_POINT('Ctrl Pts',(82.9880570189023,-0.801297825350726,3.63732405246524));
#7944=CARTESIAN_POINT('Ctrl Pts',(82.9944427688165,-0.908353516352129,3.61068347162499));
#7945=CARTESIAN_POINT('Ctrl Pts',(83.000954486814,-1.01752103452814,3.58351736708731));
#7946=CARTESIAN_POINT('Ctrl Pts',(83.0074437003446,-1.12534658989672,3.55141290154023));
#7947=CARTESIAN_POINT('Ctrl Pts',(83.0138181954763,-1.23134252417002,3.51449763874511));
#7948=CARTESIAN_POINT('Ctrl Pts',(83.0195255882697,-1.32624579398194,3.4814456243519));
#7949=CARTESIAN_POINT('Ctrl Pts',(83.0251405465292,-1.41968322053829,3.44453686041246));
#7950=CARTESIAN_POINT('Ctrl Pts',(83.0305879677352,-1.51130353807574,3.40389930429182));
#7951=CARTESIAN_POINT('Ctrl Pts',(83.03122468358,-1.52201247826612,3.39914942817618));
#7952=CARTESIAN_POINT('Ctrl Pts',(83.0318591105594,-1.53269665019523,3.3943486242449));
#7953=CARTESIAN_POINT('Ctrl Pts',(83.0324911287457,-1.5433555383646,3.38949710732856));
#7954=CARTESIAN_POINT('Ctrl Pts',(83.0324937959921,-1.54340052105906,3.38947663293202));
#7955=CARTESIAN_POINT('Ctrl Pts',(83.0324964631984,-1.54344550336794,3.38945615760467));
#7956=CARTESIAN_POINT('Ctrl Pts',(83.0324991303647,-1.54349048529117,3.38943568134652));
#7957=CARTESIAN_POINT('Ctrl Pts',(83.0378606707335,-1.63391319469024,3.34827428566594));
#7958=CARTESIAN_POINT('Ctrl Pts',(83.0430602772996,-1.72277948316394,3.30334766288235));
#7959=CARTESIAN_POINT('Ctrl Pts',(83.0481595952658,-1.80976892931888,3.25482279871221));
#7960=CARTESIAN_POINT('Ctrl Pts',(83.048771082511,-1.82020031193624,3.24900391553744));
#7961=CARTESIAN_POINT('Ctrl Pts',(83.0493811276336,-1.83060468026478,3.24313334652199));
#7962=CARTESIAN_POINT('Ctrl Pts',(83.0499898369316,-1.84098146169455,3.2372114256022));
#7963=CARTESIAN_POINT('Ctrl Pts',(83.0556710275469,-1.93782978234437,3.18194109925064));
#7964=CARTESIAN_POINT('Ctrl Pts',(83.0612364938514,-2.03227788805904,3.12219212008623));
#7965=CARTESIAN_POINT('Ctrl Pts',(83.0667674937821,-2.12391272180136,3.05824252474161));
#7966=CARTESIAN_POINT('Ctrl Pts',(83.0722929678339,-2.21545600555163,2.99435681978349));
#7967=CARTESIAN_POINT('Ctrl Pts',(83.0777844963081,-2.30419180547416,2.92627935066107));
#7968=CARTESIAN_POINT('Ctrl Pts',(83.0833097974269,-2.38974428256799,2.85431879316216));
#7969=CARTESIAN_POINT('Ctrl Pts',(83.0884653414204,-2.46957152635635,2.78717388793269));
#7970=CARTESIAN_POINT('Ctrl Pts',(83.0936503489239,-2.54662769771509,2.71664870107101));
#7971=CARTESIAN_POINT('Ctrl Pts',(83.0989050616807,-2.62063375225138,2.64301435574924));
#7972=CARTESIAN_POINT('Origin',(80.1322559480305,0.,0.));
#7973=CARTESIAN_POINT('',(84.5943437838656,-2.62112000711956,2.64359555733806));
#7974=CARTESIAN_POINT('',(84.3497092098018,-2.62112000711956,2.64359555733807));
#7975=CARTESIAN_POINT('',(80.1322559480305,-2.62112000711956,2.64359555733806));
#7976=CARTESIAN_POINT('Ctrl Pts',(84.5943437838656,-2.62112000711956,2.64359555733807));
#7977=CARTESIAN_POINT('Ctrl Pts',(84.5907408117248,-2.57694702423373,2.68739298652303));
#7978=CARTESIAN_POINT('Ctrl Pts',(84.5871743154747,-2.53166613263349,2.73009334161478));
#7979=CARTESIAN_POINT('Ctrl Pts',(84.5811736507666,-2.45240380688733,2.80116715995069));
#7980=CARTESIAN_POINT('Ctrl Pts',(84.5787120403164,-2.41896578754705,2.83009306267694));
#7981=CARTESIAN_POINT('Ctrl Pts',(84.5748329068826,-2.36462883644873,2.87543096642596));
#7982=CARTESIAN_POINT('Ctrl Pts',(84.5733911059468,-2.34405632918012,2.89222627317259));
#7983=CARTESIAN_POINT('Ctrl Pts',(84.570497528159,-2.30195399772164,2.92585407015743));
#7984=CARTESIAN_POINT('Ctrl Pts',(84.5690466230318,-2.28041520767029,2.94267239400238));
#7985=CARTESIAN_POINT('Ctrl Pts',(84.5650854642014,-2.22050570304682,2.98839919482867));
#7986=CARTESIAN_POINT('Ctrl Pts',(84.5626061580896,-2.18175658138579,3.01680525510096));
#7987=CARTESIAN_POINT('Ctrl Pts',(84.5569465167446,-2.09076601110375,3.08083783594035));
#7988=CARTESIAN_POINT('Ctrl Pts',(84.5537930363585,-2.03814459945658,3.11589979411636));
#7989=CARTESIAN_POINT('Ctrl Pts',(84.5420555568739,-1.83649143568314,3.24296702728022));
#7990=CARTESIAN_POINT('Ctrl Pts',(84.5337446102715,-1.681920586548,3.32576064655821));
#7991=CARTESIAN_POINT('Ctrl Pts',(84.5165780687902,-1.35560569201204,3.47195643619301));
#7992=CARTESIAN_POINT('Ctrl Pts',(84.5077333314623,-1.18387272711435,3.53420240092095));
#7993=CARTESIAN_POINT('Ctrl Pts',(84.495049550665,-0.942379610003741,3.60214864544964));
#7994=CARTESIAN_POINT('Ctrl Pts',(84.4915396137813,-0.875983334028462,3.6188681460994));
#7995=CARTESIAN_POINT('Ctrl Pts',(84.4858251648387,-0.768918511081819,3.64270944419393));
#7996=CARTESIAN_POINT('Ctrl Pts',(84.483657040799,-0.728525712587216,3.65100231182728));
#7997=CARTESIAN_POINT('Ctrl Pts',(84.4790522000956,-0.643282253999308,3.66703235779608));
#7998=CARTESIAN_POINT('Ctrl Pts',(84.4766113261429,-0.598410965966305,3.67462140115184));
#7999=CARTESIAN_POINT('Ctrl Pts',(84.4705284982565,-0.487423821088916,3.69130580891148));
#8000=CARTESIAN_POINT('Ctrl Pts',(84.466858368709,-0.42118283945894,3.69944925677698));
#8001=CARTESIAN_POINT('Ctrl Pts',(84.4531900791189,-0.177205120738837,3.72280554141741));
#8002=CARTESIAN_POINT('Ctrl Pts',(84.4428817201986,0.00132491966660819,
3.72701880396594));
#8003=CARTESIAN_POINT('Ctrl Pts',(84.4176185516819,0.430872740884897,3.70628865224356));
#8004=CARTESIAN_POINT('Ctrl Pts',(84.4025389352714,0.680418579246505,3.66868710253756));
#8005=CARTESIAN_POINT('Ctrl Pts',(84.3857993442423,0.967871972903168,3.59501292163595));
#8006=CARTESIAN_POINT('Ctrl Pts',(84.3832908958218,1.0112747769779,3.58304587461003));
#8007=CARTESIAN_POINT('Ctrl Pts',(84.3793566383167,1.08007433714672,3.56272659308978));
#8008=CARTESIAN_POINT('Ctrl Pts',(84.3779054069339,1.10561575140774,3.55488329816625));
#8009=CARTESIAN_POINT('Ctrl Pts',(84.3750120735372,1.15692516796013,3.53852061059081));
#8010=CARTESIAN_POINT('Ctrl Pts',(84.3735704836368,1.18268877458042,3.52999310297551));
#8011=CARTESIAN_POINT('Ctrl Pts',(84.369666264972,1.25291181379502,3.50589480711796));
#8012=CARTESIAN_POINT('Ctrl Pts',(84.3672331218709,1.29717376505416,3.48976030941729));
#8013=CARTESIAN_POINT('Ctrl Pts',(84.3617017477928,1.39851141047655,3.45062580757112));
#8014=CARTESIAN_POINT('Ctrl Pts',(84.3586286512319,1.45534754903912,3.42704198262726));
#8015=CARTESIAN_POINT('Ctrl Pts',(84.3474319657509,1.66283855011653,3.33485127933889));
#8016=CARTESIAN_POINT('Ctrl Pts',(84.3395572551233,1.80945719461367,3.25762708242629));
#8017=CARTESIAN_POINT('Ctrl Pts',(84.3222785632027,2.11635843277074,3.06884879462024));
#8018=CARTESIAN_POINT('Ctrl Pts',(84.3128680198459,2.27398901790162,2.95394178383975));
#8019=CARTESIAN_POINT('Ctrl Pts',(84.2995485779715,2.47411337241145,2.78250926605326));
#8020=CARTESIAN_POINT('Ctrl Pts',(84.296024258384,2.52507775260058,2.7363436182026));
#8021=CARTESIAN_POINT('Ctrl Pts',(84.2900547733815,2.60784893114347,2.65708370246044));
#8022=CARTESIAN_POINT('Ctrl Pts',(84.2876417712766,2.6403753795398,2.62476426777186));
#8023=CARTESIAN_POINT('Ctrl Pts',(84.2827389293107,2.70454585537788,2.55860215444187));
#8024=CARTESIAN_POINT('Ctrl Pts',(84.2802489902953,2.73617154133603,2.52475311775694));
#8025=CARTESIAN_POINT('Ctrl Pts',(84.2738535020615,2.81492993130633,2.43723968187162));
#8026=CARTESIAN_POINT('Ctrl Pts',(84.2699130170268,2.86116356024535,2.38279456297719));
#8027=CARTESIAN_POINT('Ctrl Pts',(84.2610516127332,2.96010191291042,2.2592499810353));
#8028=CARTESIAN_POINT('Ctrl Pts',(84.2561055503558,3.01201010057387,2.18956787623521));
#8029=CARTESIAN_POINT('Ctrl Pts',(84.2384670572311,3.18596455336875,1.93814433452625));
#8030=CARTESIAN_POINT('Ctrl Pts',(84.2254299849798,3.29437700720137,1.74752503198462));
#8031=CARTESIAN_POINT('Ctrl Pts',(84.2050634053166,3.43866463914452,1.43207700898199));
#8032=CARTESIAN_POINT('Ctrl Pts',(84.197632015305,3.48588192004519,1.31297034717319));
#8033=CARTESIAN_POINT('Ctrl Pts',(84.1883292545763,3.53907756980524,1.15553096761608));
#8034=CARTESIAN_POINT('Ctrl Pts',(84.186218585374,3.55072936347778,1.11921538327329));
#8035=CARTESIAN_POINT('Ctrl Pts',(84.1827469091141,3.56923052915444,1.05835246769119));
#8036=CARTESIAN_POINT('Ctrl Pts',(84.1813699096741,3.5763894418461,1.03390290296337));
#8037=CARTESIAN_POINT('Ctrl Pts',(84.1784375573012,3.59125482878852,0.981130805707437));
#8038=CARTESIAN_POINT('Ctrl Pts',(84.1768865136219,3.5988782753272,0.952787579275031));
#8039=CARTESIAN_POINT('Ctrl Pts',(84.1722852675025,3.62072785824913,0.867546396624193));
#8040=CARTESIAN_POINT('Ctrl Pts',(84.1692846266782,3.63394601047137,0.810397464662491));
#8041=CARTESIAN_POINT('Ctrl Pts',(84.1621020064946,3.6628001218698,0.670686262505496));
#8042=CARTESIAN_POINT('Ctrl Pts',(84.1579720029296,3.6770024320648,0.587859811889969));
#8043=CARTESIAN_POINT('Ctrl Pts',(84.1467325117819,3.70836212673273,0.358644363935539));
#8044=CARTESIAN_POINT('Ctrl Pts',(84.139729669639,3.71965033175558,0.211609151992778));
#8045=CARTESIAN_POINT('Ctrl Pts',(84.124338503213,3.72518013950449,-0.108550759841699));
#8046=CARTESIAN_POINT('Ctrl Pts',(84.1159340985949,3.71612293617322,-0.28137920340409));
#8047=CARTESIAN_POINT('Ctrl Pts',(84.1037517379495,3.68681766587235,-0.520450600870952));
#8048=CARTESIAN_POINT('Ctrl Pts',(84.1002635525532,3.67669451779837,-0.587715945053337));
#8049=CARTESIAN_POINT('Ctrl Pts',(84.0945748802005,3.65749669436818,-0.695183219553958));
#8050=CARTESIAN_POINT('Ctrl Pts',(84.0924101336644,3.64958704759242,-0.735578673081256));
#8051=CARTESIAN_POINT('Ctrl Pts',(84.0878047246451,3.63151184317475,-0.82040612110599));
#8052=CARTESIAN_POINT('Ctrl Pts',(84.0853597564598,3.62119688769866,-0.864799008206719));
#8053=CARTESIAN_POINT('Ctrl Pts',(84.0792494618808,3.59367471008639,-0.97410381368601));
#8054=CARTESIAN_POINT('Ctrl Pts',(84.0755553717232,3.57552166738603,-1.03875896391701));
#8055=CARTESIAN_POINT('Ctrl Pts',(84.0617433431509,3.50217466392701,-1.27522498261098));
#8056=CARTESIAN_POINT('Ctrl Pts',(84.0513076660164,3.4362649717634,-1.44343236607213));
#8057=CARTESIAN_POINT('Ctrl Pts',(84.0261620472898,3.25166356077067,-1.82942232898161));
#8058=CARTESIAN_POINT('Ctrl Pts',(84.0113476991096,3.12290440216804,-2.04146461653696));
#8059=CARTESIAN_POINT('Ctrl Pts',(83.9947986877853,2.9465686835436,-2.27567326465751));
#8060=CARTESIAN_POINT('Ctrl Pts',(83.992250802565,2.91841143345712,-2.31167274615398));
#8061=CARTESIAN_POINT('Ctrl Pts',(83.9882700771743,2.87266631583368,-2.36799006048822));
#8062=CARTESIAN_POINT('Ctrl Pts',(83.9868108414173,2.85550974501347,-2.3886508491862));
#8063=CARTESIAN_POINT('Ctrl Pts',(83.9839162008507,2.82065474515235,-2.42971266479577));
#8064=CARTESIAN_POINT('Ctrl Pts',(83.9824810306217,2.80295490985435,-2.45011034154927));
#8065=CARTESIAN_POINT('Ctrl Pts',(83.9786184637149,2.75423620677078,-2.50503584506203));
#8066=CARTESIAN_POINT('Ctrl Pts',(83.9762194626911,2.72279029923352,-2.53917998995266));
#8067=CARTESIAN_POINT('Ctrl Pts',(83.9657025807219,2.58016693270706,-2.68834400357289));
#8068=CARTESIAN_POINT('Ctrl Pts',(83.9579573855615,2.46227521480837,-2.79672371871057));
#8069=CARTESIAN_POINT('Ctrl Pts',(83.9372898075075,2.12742924115124,-3.06691400402808));
#8070=CARTESIAN_POINT('Ctrl Pts',(83.9244850361729,1.8992498215517,-3.21321606987893));
#8071=CARTESIAN_POINT('Ctrl Pts',(83.9074654178086,1.59864549381558,-3.36266012016666));
#8072=CARTESIAN_POINT('Ctrl Pts',(83.9041022933889,1.53928811529006,-3.39024216673092));
#8073=CARTESIAN_POINT('Ctrl Pts',(83.8983470982289,1.43807697698841,-3.43406667482501));
#8074=CARTESIAN_POINT('Ctrl Pts',(83.8959829439032,1.39659974414915,-3.4511430345628));
#8075=CARTESIAN_POINT('Ctrl Pts',(83.8910911230138,1.31105541559054,-3.48456733821529));
#8076=CARTESIAN_POINT('Ctrl Pts',(83.888561483009,1.26696713146479,-3.50083845017561));
#8077=CARTESIAN_POINT('Ctrl Pts',(83.8819218464268,1.15169707818524,-3.54091708785826));
#8078=CARTESIAN_POINT('Ctrl Pts',(83.8777714063153,1.08008484838386,-3.5634134787781));
#8079=CARTESIAN_POINT('Ctrl Pts',(83.8620761086517,0.810961695344269,-3.63909843807001));
#8080=CARTESIAN_POINT('Ctrl Pts',(83.850130364349,0.609870390883411,-3.67814332495648));
#8081=CARTESIAN_POINT('Ctrl Pts',(83.8256650263185,0.197744638436171,-3.72342813404117));
#8082=CARTESIAN_POINT('Ctrl Pts',(83.813185547929,-0.0127021723266912,-3.72865502766819));
#8083=CARTESIAN_POINT('Ctrl Pts',(83.7988497881874,-0.266593216618914,-3.71345513873554));
#8084=CARTESIAN_POINT('Ctrl Pts',(83.7963887885953,-0.31066345018899,-3.71002824325117));
#8085=CARTESIAN_POINT('Ctrl Pts',(83.7925102324633,-0.381099794141748,-3.70328715616226));
#8086=CARTESIAN_POINT('Ctrl Pts',(83.7910684184602,-0.407508778907855,-3.70047422913305));
#8087=CARTESIAN_POINT('Ctrl Pts',(83.7881754169206,-0.461015345136506,-3.6941952474613));
#8088=CARTESIAN_POINT('Ctrl Pts',(83.7867250952236,-0.488109207155726,-3.69071309735153));
#8089=CARTESIAN_POINT('Ctrl Pts',(83.7827650493563,-0.562731015880428,-3.68028643574708));
#8090=CARTESIAN_POINT('Ctrl Pts',(83.7802862832299,-0.610167954686656,-3.67271968916089));
#8091=CARTESIAN_POINT('Ctrl Pts',(83.7746277565682,-0.719664287696303,-3.65307356352266));
#8092=CARTESIAN_POINT('Ctrl Pts',(83.7714748625238,-0.781589598965452,-3.64032711402842));
#8093=CARTESIAN_POINT('Ctrl Pts',(83.7597393768794,-1.01371713957767,-3.58635006999138));
#8094=CARTESIAN_POINT('Ctrl Pts',(83.7514299816506,-1.18126728001109,-3.53470531796971));
#8095=CARTESIAN_POINT('Ctrl Pts',(83.734262346508,-1.51474822161404,-3.40554144912009));
#8096=CARTESIAN_POINT('Ctrl Pts',(83.7254148637551,-1.67984427710116,-3.32720466609754));
#8097=CARTESIAN_POINT('Ctrl Pts',(83.7127286246209,-1.89803730029192,-3.20328063003238));
#8098=CARTESIAN_POINT('Ctrl Pts',(83.7092194914655,-1.9566075785217,-3.16784444675353));
#8099=CARTESIAN_POINT('Ctrl Pts',(83.7035068916617,-2.04882692839932,-3.10851643418255));
#8100=CARTESIAN_POINT('Ctrl Pts',(83.7013398295392,-2.08311454545353,-3.08564414963074));
#8101=CARTESIAN_POINT('Ctrl Pts',(83.6967378012349,-2.15442032686303,-3.03634789720623));
#8102=CARTESIAN_POINT('Ctrl Pts',(83.6942986904656,-2.19134800058597,-3.00980550749131));
#8103=CARTESIAN_POINT('Ctrl Pts',(83.6882217606141,-2.28118322692421,-2.94270517858672));
#8104=CARTESIAN_POINT('Ctrl Pts',(83.6845558307243,-2.3335038180017,-2.90139101944681));
#8105=CARTESIAN_POINT('Ctrl Pts',(83.6709156615242,-2.52133057801611,-2.74470852758297));
#8106=CARTESIAN_POINT('Ctrl Pts',(83.6606325783451,-2.64961333819856,-2.62108187054481));
#8107=CARTESIAN_POINT('Ctrl Pts',(83.6353445582929,-2.93740380228922,-2.30093834212829));
#8108=CARTESIAN_POINT('Ctrl Pts',(83.6202104524724,-3.08670336957429,-2.09640841368864));
#8109=CARTESIAN_POINT('Ctrl Pts',(83.6034323350909,-3.23678601111543,-1.83959163132951));
#8110=CARTESIAN_POINT('Ctrl Pts',(83.600932154433,-3.25872507627587,-1.80044224502325));
#8111=CARTESIAN_POINT('Ctrl Pts',(83.5970082250196,-3.29257027843675,-1.73740040696266));
#8112=CARTESIAN_POINT('Ctrl Pts',(83.5955592352651,-3.30493615877901,-1.71376086497502));
#8113=CARTESIAN_POINT('Ctrl Pts',(83.5926682289649,-3.32936576094034,-1.66581137076539));
#8114=CARTESIAN_POINT('Ctrl Pts',(83.5912267649167,-3.34141987400688,-1.64149846404188));
#8115=CARTESIAN_POINT('Ctrl Pts',(83.5873199974801,-3.37369151385901,-1.57457836004272));
#8116=CARTESIAN_POINT('Ctrl Pts',(83.5848842973406,-3.39336753313681,-1.53171427209088));
#8117=CARTESIAN_POINT('Ctrl Pts',(83.5793456764399,-3.43686380337712,-1.43200286514232));
#8118=CARTESIAN_POINT('Ctrl Pts',(83.576268019616,-3.46009776651618,-1.37491420388966));
#8119=CARTESIAN_POINT('Ctrl Pts',(83.5650427675964,-3.54065691283645,-1.16197483124453));
#8120=CARTESIAN_POINT('Ctrl Pts',(83.557145716562,-3.58895597481763,-1.00291394112117));
#8121=CARTESIAN_POINT('Ctrl Pts',(83.5398542127997,-3.67044132321864,-0.651605608013829));
#8122=CARTESIAN_POINT('Ctrl Pts',(83.5304535338369,-3.69947586432838,-0.458911618107906));
#8123=CARTESIAN_POINT('Ctrl Pts',(83.5171433971881,-3.71821063906794,-0.196235217835148));
#8124=CARTESIAN_POINT('Ctrl Pts',(83.5136177975025,-3.72120138402812,-0.127507387027372));
#8125=CARTESIAN_POINT('Ctrl Pts',(83.5076470622219,-3.72301000902447,-0.012894329024348));
#8126=CARTESIAN_POINT('Ctrl Pts',(83.5052341495047,-3.72288642235409,0.0329580629838045));
#8127=CARTESIAN_POINT('Ctrl Pts',(83.5003324123124,-3.72093596767528,0.125088397827464));
#8128=CARTESIAN_POINT('Ctrl Pts',(83.4978435081746,-3.71909233999502,0.171357784670287));
#8129=CARTESIAN_POINT('Ctrl Pts',(83.491452845202,-3.71221623529657,0.288805760694303));
#8130=CARTESIAN_POINT('Ctrl Pts',(83.4875162445366,-3.70599967245431,0.359893926441016));
#8131=CARTESIAN_POINT('Ctrl Pts',(83.478664832102,-3.68770504074861,0.516940606885447));
#8132=CARTESIAN_POINT('Ctrl Pts',(83.4737249643479,-3.67465587394784,0.60274272375685));
#8133=CARTESIAN_POINT('Ctrl Pts',(83.4561240780356,-3.61826802281,0.902597144908889));
#8134=CARTESIAN_POINT('Ctrl Pts',(83.4431202777285,-3.55911362452114,1.11321397400137));
#8135=CARTESIAN_POINT('Ctrl Pts',(83.4227559890907,-3.43637599911366,1.43760235292464));
#8136=CARTESIAN_POINT('Ctrl Pts',(83.4152964168224,-3.38470505817501,1.55536396712365));
#8137=CARTESIAN_POINT('Ctrl Pts',(83.4059646572083,-3.3099141267479,1.70434552948618));
#8138=CARTESIAN_POINT('Ctrl Pts',(83.4038515566164,-3.29226035821143,1.73820228088201));
#8139=CARTESIAN_POINT('Ctrl Pts',(83.400375277444,-3.26194459398117,1.79422296840556));
#8140=CARTESIAN_POINT('Ctrl Pts',(83.3989961122763,-3.24957023338223,1.81653847426224));
#8141=CARTESIAN_POINT('Ctrl Pts',(83.3960545490362,-3.2224056020191,1.8643601574954));
#8142=CARTESIAN_POINT('Ctrl Pts',(83.3944965561383,-3.20754028295992,1.88982065381401));
#8143=CARTESIAN_POINT('Ctrl Pts',(83.3898687214094,-3.16200993093883,1.96571731311643));
#8144=CARTESIAN_POINT('Ctrl Pts',(83.3868488959017,-3.13044526266745,2.01560524622334));
#8145=CARTESIAN_POINT('Ctrl Pts',(83.3712610487424,-2.95873247827631,2.27322601385967));
#8146=CARTESIAN_POINT('Ctrl Pts',(83.3595107797603,-2.79905425345494,2.46717808435461));
#8147=CARTESIAN_POINT('Ctrl Pts',(83.3474186374517,-2.62109006714222,2.6436252424329));
#8148=CARTESIAN_POINT('Ctrl Pts',(83.098469847874,-2.62118125581997,2.64353482796011));
#8149=CARTESIAN_POINT('Ctrl Pts',(83.1019574372931,-2.67139426381132,2.59374641815623));
#8150=CARTESIAN_POINT('Ctrl Pts',(83.1054855024516,-2.72017682180231,2.5425391353066));
#8151=CARTESIAN_POINT('Ctrl Pts',(83.1118033862382,-2.80360914658851,2.4498087036034));
#8152=CARTESIAN_POINT('Ctrl Pts',(83.1145701895591,-2.83886818604681,2.40886155681767));
#8153=CARTESIAN_POINT('Ctrl Pts',(83.1195489931295,-2.8999395055749,2.3347342098428));
#8154=CARTESIAN_POINT('Ctrl Pts',(83.1217471863391,-2.92610477278024,2.30185656464413));
#8155=CARTESIAN_POINT('Ctrl Pts',(83.1263428990979,-2.97912168747791,2.23287380698539));
#8156=CARTESIAN_POINT('Ctrl Pts',(83.1287431365892,-3.00588638764174,2.19671078212789));
#8157=CARTESIAN_POINT('Ctrl Pts',(83.1342900267089,-3.06560342990674,2.11288888582904));
#8158=CARTESIAN_POINT('Ctrl Pts',(83.1374519743175,-3.09811109853042,2.06492880281431));
#8159=CARTESIAN_POINT('Ctrl Pts',(83.148563313287,-3.20703996006023,1.89585531750673));
#8160=CARTESIAN_POINT('Ctrl Pts',(83.1567055502609,-3.27757770863589,1.77111562965551));
#8161=CARTESIAN_POINT('Ctrl Pts',(83.1805745818944,-3.45938957611759,1.40135064081698));
#8162=CARTESIAN_POINT('Ctrl Pts',(83.1966664659931,-3.55153455995938,1.14793606527946));
#8163=CARTESIAN_POINT('Ctrl Pts',(83.2154312749336,-3.62998102702292,0.828105769791334));
#8164=CARTESIAN_POINT('Ctrl Pts',(83.2188306246917,-3.64294917084279,0.769053639683291));
#8165=CARTESIAN_POINT('Ctrl Pts',(83.2238258012988,-3.66021377351113,0.68015377327869));
#8166=CARTESIAN_POINT('Ctrl Pts',(83.2254702006369,-3.6655949308124,0.650528970569234));
#8167=CARTESIAN_POINT('Ctrl Pts',(83.2284883555675,-3.67491787875769,0.595408655076993));
#8168=CARTESIAN_POINT('Ctrl Pts',(83.229866451666,-3.67895484388861,0.569933479859903));
#8169=CARTESIAN_POINT('Ctrl Pts',(83.2332792816183,-3.68838969010322,0.50611107267406));
#8170=CARTESIAN_POINT('Ctrl Pts',(83.2352971474211,-3.69345457936936,0.467718311521839));
#8171=CARTESIAN_POINT('Ctrl Pts',(83.2444837245172,-3.71403965283023,0.290382084915086));
#8172=CARTESIAN_POINT('Ctrl Pts',(83.2513439070078,-3.72232551954412,0.150702549098464));
#8173=CARTESIAN_POINT('Ctrl Pts',(83.2681919147471,-3.72334351390773,-0.197669853681005));
#8174=CARTESIAN_POINT('Ctrl Pts',(83.2780459464207,-3.70642792281704,-0.40589729167305));
#8175=CARTESIAN_POINT('Ctrl Pts',(83.292421391106,-3.65820856846187,-0.695409382260557));
#8176=CARTESIAN_POINT('Ctrl Pts',(83.2966342957239,-3.64138841968838,-0.778699848403936));
#8177=CARTESIAN_POINT('Ctrl Pts',(83.3044683116323,-3.60549424227617,-0.929626687793152));
#8178=CARTESIAN_POINT('Ctrl Pts',(83.3080633501534,-3.58732638734039,-0.997438277824222));
#8179=CARTESIAN_POINT('Ctrl Pts',(83.314110590084,-3.55410677265165,-1.10874054839327));
#8180=CARTESIAN_POINT('Ctrl Pts',(83.3165284428942,-3.54014600293421,-1.15253919173449));
#8181=CARTESIAN_POINT('Ctrl Pts',(83.3214072886937,-3.51066315906593,-1.23943916059089));
#8182=CARTESIAN_POINT('Ctrl Pts',(83.3238676693217,-3.49514942245258,-1.2825348000298));
#8183=CARTESIAN_POINT('Ctrl Pts',(83.3301111863393,-3.45420154760582,-1.3900182892505));
#8184=CARTESIAN_POINT('Ctrl Pts',(83.333926226665,-3.42775991629598,-1.45400146985651));
#8185=CARTESIAN_POINT('Ctrl Pts',(83.3507392181853,-3.30519712661945,-1.72862338649515));
#8186=CARTESIAN_POINT('Ctrl Pts',(83.3643000622881,-3.19133799317504,-1.93075235536862));
#8187=CARTESIAN_POINT('Ctrl Pts',(83.3863460441463,-2.97886377352015,-2.23724221252285));
#8188=CARTESIAN_POINT('Ctrl Pts',(83.3947256290841,-2.89169761274429,-2.34882298150625));
#8189=CARTESIAN_POINT('Ctrl Pts',(83.4061974553829,-2.760946539539,-2.49785211217532));
#8190=CARTESIAN_POINT('Ctrl Pts',(83.4094494683065,-2.72253007393496,-2.53966956415872));
#8191=CARTESIAN_POINT('Ctrl Pts',(83.4151561746597,-2.65239991395943,-2.61258735767042));
#8192=CARTESIAN_POINT('Ctrl Pts',(83.4176295487401,-2.62105805935229,-2.6440296887582));
#8193=CARTESIAN_POINT('Ctrl Pts',(83.4215150864135,-2.57015340313916,-2.69330257512577));
#8194=CARTESIAN_POINT('Ctrl Pts',(83.4229520449323,-2.55095057477377,-2.71149747168903));
#8195=CARTESIAN_POINT('Ctrl Pts',(83.425816422974,-2.51186452435651,-2.74774915063062));
#8196=CARTESIAN_POINT('Ctrl Pts',(83.4272433384157,-2.49197664028869,-2.76579849128174));
#8197=CARTESIAN_POINT('Ctrl Pts',(83.4311030039209,-2.43710763392315,-2.81452275537215));
#8198=CARTESIAN_POINT('Ctrl Pts',(83.4335068401291,-2.40174315669938,-2.84476047159436));
#8199=CARTESIAN_POINT('Ctrl Pts',(83.4448235231234,-2.23020048565785,-2.98595484667776));
#8200=CARTESIAN_POINT('Ctrl Pts',(83.4532786251432,-2.08683938004369,-3.08785232799685));
#8201=CARTESIAN_POINT('Ctrl Pts',(83.4729921981318,-1.73555161988876,-3.30185778333071));
#8202=CARTESIAN_POINT('Ctrl Pts',(83.4842041296979,-1.523112111121,-3.40507356551663));
#8203=CARTESIAN_POINT('Ctrl Pts',(83.4997954177205,-1.23264609126699,-3.51354357105568));
#8204=CARTESIAN_POINT('Ctrl Pts',(83.5035931954064,-1.16217390122115,-3.53747872251818));
#8205=CARTESIAN_POINT('Ctrl Pts',(83.5098753902681,-1.04652385111574,-3.57292915595346));
#8206=CARTESIAN_POINT('Ctrl Pts',(83.5123186107983,-1.00176250625304,-3.58573654238083));
#8207=CARTESIAN_POINT('Ctrl Pts',(83.517142338507,-0.91390086306699,-3.60910250353065));
#8208=CARTESIAN_POINT('Ctrl Pts',(83.5195199898844,-0.87082865412088,-3.6197365781609));
#8209=CARTESIAN_POINT('Ctrl Pts',(83.5254148154727,-0.764678367436689,-3.64393970715429));
#8210=CARTESIAN_POINT('Ctrl Pts',(83.5289580955598,-0.70141954670096,-3.65664320313402));
#8211=CARTESIAN_POINT('Ctrl Pts',(83.5479238615281,-0.365804543954081,-3.71501147973908));
#8212=CARTESIAN_POINT('Ctrl Pts',(83.5642139243494,-0.0893565686471371,
-3.73190275534186));
#8213=CARTESIAN_POINT('Ctrl Pts',(83.5898004013558,0.343430837968755,-3.71020935333544));
#8214=CARTESIAN_POINT('Ctrl Pts',(83.5990423818078,0.499847423044,-3.69239179482749));
#8215=CARTESIAN_POINT('Ctrl Pts',(83.6105203297548,0.699897332124375,-3.65665441007835));
#8216=CARTESIAN_POINT('Ctrl Pts',(83.613082837461,0.744966860825984,-3.64773936833899));
#8217=CARTESIAN_POINT('Ctrl Pts',(83.6170720108416,0.815994442913929,-3.63231823246569));
#8218=CARTESIAN_POINT('Ctrl Pts',(83.618525703413,0.842066165854466,-3.6263628257679));
#8219=CARTESIAN_POINT('Ctrl Pts',(83.6214004812374,0.89406154780247,-3.61389482242231));
#8220=CARTESIAN_POINT('Ctrl Pts',(83.6228215560301,0.919983667154045,-3.60738298162023));
#8221=CARTESIAN_POINT('Ctrl Pts',(83.6266150080844,0.989681143346163,-3.58907425670544));
#8222=CARTESIAN_POINT('Ctrl Pts',(83.628960595293,1.0333159162256,-3.57675570138799));
#8223=CARTESIAN_POINT('Ctrl Pts',(83.6414295033508,1.26726159059395,-3.50607151516963));
#8224=CARTESIAN_POINT('Ctrl Pts',(83.6509518726035,1.45289962882292,-3.43330539136195));
#8225=CARTESIAN_POINT('Ctrl Pts',(83.6681803098899,1.77605319751593,-3.27570547661866));
#8226=CARTESIAN_POINT('Ctrl Pts',(83.6758611411785,1.91556437078074,-3.19612605474789));
#8227=CARTESIAN_POINT('Ctrl Pts',(83.6874804758913,2.11227274049254,-3.0664026497785));
#8228=CARTESIAN_POINT('Ctrl Pts',(83.6912346145942,2.17377257973285,-3.02311648994599));
#8229=CARTESIAN_POINT('Ctrl Pts',(83.6983168891236,2.28540184073791,-2.93937887298271));
#8230=CARTESIAN_POINT('Ctrl Pts',(83.7016271970787,2.33587384168366,-2.89943141161603));
#8231=CARTESIAN_POINT('Ctrl Pts',(83.7073396816165,2.41987311922688,-2.82933055505599));
#8232=CARTESIAN_POINT('Ctrl Pts',(83.7097158835423,2.45393504357483,-2.79983925849361));
#8233=CARTESIAN_POINT('Ctrl Pts',(83.7146355616783,2.52261031264785,-2.73816321795688));
#8234=CARTESIAN_POINT('Ctrl Pts',(83.7171810826185,2.55716264979442,-2.70592304127606));
#8235=CARTESIAN_POINT('Ctrl Pts',(83.7239392847304,2.64629262550365,-2.61952541337996));
#8236=CARTESIAN_POINT('Ctrl Pts',(83.7281952601577,2.69982054700934,-2.56432172474487));
#8237=CARTESIAN_POINT('Ctrl Pts',(83.7499826356791,2.96089874615753,-2.27782858776448));
#8238=CARTESIAN_POINT('Ctrl Pts',(83.7685664557161,3.14060217549853,-2.02286790716614));
#8239=CARTESIAN_POINT('Ctrl Pts',(83.7913395222776,3.32348096114568,-1.67914658047097));
#8240=CARTESIAN_POINT('Ctrl Pts',(83.7959013647612,3.35823024278104,-1.6085240608104));
#8241=CARTESIAN_POINT('Ctrl Pts',(83.8035730927915,3.41385405435936,-1.48580257627947));
#8242=CARTESIAN_POINT('Ctrl Pts',(83.8067219968625,3.43583708250895,-1.43423602341418));
#8243=CARTESIAN_POINT('Ctrl Pts',(83.8114037481945,3.46736274461901,-1.3553951230656));
#8244=CARTESIAN_POINT('Ctrl Pts',(83.8129792869184,3.47776559100389,-1.32847542011444));
#8245=CARTESIAN_POINT('Ctrl Pts',(83.8159006747901,3.49668773279909,-1.27776401491703));
#8246=CARTESIAN_POINT('Ctrl Pts',(83.8172501709169,3.50527947070012,-1.25400232286149));
#8247=CARTESIAN_POINT('Ctrl Pts',(83.8206378283228,3.52644405165829,-1.19355098730942));
#8248=CARTESIAN_POINT('Ctrl Pts',(83.8226583233178,3.53868700655612,-1.15674807351858));
#8249=CARTESIAN_POINT('Ctrl Pts',(83.832175310705,3.59433678777667,-0.980302663840718));
#8250=CARTESIAN_POINT('Ctrl Pts',(83.8393301461734,3.63006939470891,-0.838363577227186));
#8251=CARTESIAN_POINT('Ctrl Pts',(83.8591030060327,3.70652575609342,-0.43583518847978));
#8252=CARTESIAN_POINT('Ctrl Pts',(83.8714977090779,3.72807209196568,-0.172514621926704));
#8253=CARTESIAN_POINT('Ctrl Pts',(83.8888317027794,3.71960678134602,0.174170126791537));
#8254=CARTESIAN_POINT('Ctrl Pts',(83.8930627672214,3.71477717642392,0.257369625331266));
#8255=CARTESIAN_POINT('Ctrl Pts',(83.8998792990313,3.70274152684063,0.388470659618078));
#8256=CARTESIAN_POINT('Ctrl Pts',(83.9024091253234,3.69738531732284,0.436515523721091));
#8257=CARTESIAN_POINT('Ctrl Pts',(83.9073165782005,3.68532016697538,0.528443356015807));
#8258=CARTESIAN_POINT('Ctrl Pts',(83.9096892948221,3.67875885246777,0.572337480869173));
#8259=CARTESIAN_POINT('Ctrl Pts',(83.9153561201397,3.66139506238959,0.675809973773638));
#8260=CARTESIAN_POINT('Ctrl Pts',(83.9186702680425,3.64992094283978,0.735261488809868));
#8261=CARTESIAN_POINT('Ctrl Pts',(83.9321545299543,3.5980313441256,0.972826353178651));
#8262=CARTESIAN_POINT('Ctrl Pts',(83.9426699958443,3.54598801609364,1.14811863760818));
#8263=CARTESIAN_POINT('Ctrl Pts',(83.9644612541729,3.41438841777966,1.4954905599786));
#8264=CARTESIAN_POINT('Ctrl Pts',(83.9757187198851,3.33413283906783,1.66676284064558));
#8265=CARTESIAN_POINT('Ctrl Pts',(83.9905065180707,3.20904654541324,1.88816522702087));
#8266=CARTESIAN_POINT('Ctrl Pts',(83.9942737545092,3.17536818971835,1.94426984887022));
#8267=CARTESIAN_POINT('Ctrl Pts',(84.0007659516136,3.11380640399068,2.04095495915585));
#8268=CARTESIAN_POINT('Ctrl Pts',(84.0035169292162,3.08656435114939,2.08192421076682));
#8269=CARTESIAN_POINT('Ctrl Pts',(84.0077316415476,3.04285854452846,2.14490881709202));
#8270=CARTESIAN_POINT('Ctrl Pts',(84.0092270970168,3.02695028868626,2.16730108620656));
#8271=CARTESIAN_POINT('Ctrl Pts',(84.0121155207422,2.99539878649255,2.21068743945296));
#8272=CARTESIAN_POINT('Ctrl Pts',(84.0135096803278,2.97977931604068,2.2316962412152));
#8273=CARTESIAN_POINT('Ctrl Pts',(84.0171429198265,2.93808905233098,2.2865531897942));
#8274=CARTESIAN_POINT('Ctrl Pts',(84.0193589832969,2.91165415692369,2.3201213619577));
#8275=CARTESIAN_POINT('Ctrl Pts',(84.0331645001209,2.74112215983529,2.52916375302575));
#8276=CARTESIAN_POINT('Ctrl Pts',(84.043938514612,2.58178926431126,2.69161738540142));
#8277=CARTESIAN_POINT('Ctrl Pts',(84.0640354844138,2.26206594690381,2.96291647623786));
#8278=CARTESIAN_POINT('Ctrl Pts',(84.0732971670363,2.10609487571415,3.07573956171173));
#8279=CARTESIAN_POINT('Ctrl Pts',(84.0866913559062,1.87902215522718,3.21459380845086));
#8280=CARTESIAN_POINT('Ctrl Pts',(84.0904684399076,1.81479155741648,3.25128717766199));
#8281=CARTESIAN_POINT('Ctrl Pts',(84.0967333798635,1.70836221644715,3.30795095421422));
#8282=CARTESIAN_POINT('Ctrl Pts',(84.099181069804,1.66680456630133,3.32908444794027));
#8283=CARTESIAN_POINT('Ctrl Pts',(84.1040267765092,1.5846661436843,3.36893109695096));
#8284=CARTESIAN_POINT('Ctrl Pts',(84.106422208452,1.54412359661742,3.38770506523166));
#8285=CARTESIAN_POINT('Ctrl Pts',(84.1123890302334,1.44334814511332,3.43218612408494));
#8286=CARTESIAN_POINT('Ctrl Pts',(84.1159875648216,1.38275769995227,3.45704149152967));
#8287=CARTESIAN_POINT('Ctrl Pts',(84.1346231266302,1.07004593541259,3.57578547106133));
#8288=CARTESIAN_POINT('Ctrl Pts',(84.1504697163957,0.808964811985726,3.64373144742515));
#8289=CARTESIAN_POINT('Ctrl Pts',(84.1733607915825,0.425332188804449,3.70028102280097));
#8290=CARTESIAN_POINT('Ctrl Pts',(84.1803548463131,0.307009869683719,3.71197174011133));
#8291=CARTESIAN_POINT('Ctrl Pts',(84.1901691407294,0.136813023962568,3.72059273318745));
#8292=CARTESIAN_POINT('Ctrl Pts',(84.1931099819025,0.0852480139100827,3.72213128235171));
#8293=CARTESIAN_POINT('Ctrl Pts',(84.1983339857973,-0.00770359895059893,
3.72297190193208));
#8294=CARTESIAN_POINT('Ctrl Pts',(84.2006317234332,-0.0490780697114772,
3.7226564105393));
#8295=CARTESIAN_POINT('Ctrl Pts',(84.2043143133982,-0.116360698631534,3.72102136698503));
#8296=CARTESIAN_POINT('Ctrl Pts',(84.2057196035041,-0.142274944869516,3.72012066996029));
#8297=CARTESIAN_POINT('Ctrl Pts',(84.2086055589493,-0.196043761138974,3.7176891255887));
#8298=CARTESIAN_POINT('Ctrl Pts',(84.2100840944507,-0.223894252864475,3.71611585521241));
#8299=CARTESIAN_POINT('Ctrl Pts',(84.2142380780444,-0.302891348751411,3.7107619683436));
#8300=CARTESIAN_POINT('Ctrl Pts',(84.2168772113505,-0.353982673149821,3.70623721594947));
#8301=CARTESIAN_POINT('Ctrl Pts',(84.2312323793825,-0.635473455039668,3.67543341903601));
#8302=CARTESIAN_POINT('Ctrl Pts',(84.2421805545492,-0.86313900884722,3.62872521974366));
#8303=CARTESIAN_POINT('Ctrl Pts',(84.2628928456695,-1.27586437786784,3.50297750772648));
#8304=CARTESIAN_POINT('Ctrl Pts',(84.272575472588,-1.46173922906316,3.42957582697454));
#8305=CARTESIAN_POINT('Ctrl Pts',(84.2858448571129,-1.69572079643334,3.31468530409074));
#8306=CARTESIAN_POINT('Ctrl Pts',(84.2889984231363,-1.74994183526802,3.28638261928115));
#8307=CARTESIAN_POINT('Ctrl Pts',(84.2945241585787,-1.84235607058178,3.23520796849765));
#8308=CARTESIAN_POINT('Ctrl Pts',(84.296874523898,-1.88088225065286,3.21296253094685));
#8309=CARTESIAN_POINT('Ctrl Pts',(84.3018192865424,-1.9602531737934,3.16521607253678));
#8310=CARTESIAN_POINT('Ctrl Pts',(84.3044173862902,-2.00102017821013,3.13960240254245));
#8311=CARTESIAN_POINT('Ctrl Pts',(84.3115244655315,-2.10996688056973,3.06816785156896));
#8312=CARTESIAN_POINT('Ctrl Pts',(84.3160856508743,-2.17714262819681,3.02087119439549));
#8313=CARTESIAN_POINT('Ctrl Pts',(84.3301561047506,-2.37617875549688,2.87064624215964));
#8314=CARTESIAN_POINT('Ctrl Pts',(84.3398805274516,-2.50259335409639,2.76111451017243));
#8315=CARTESIAN_POINT('Ctrl Pts',(84.3497092098018,-2.62112000711955,2.64359555733807));
#8316=CARTESIAN_POINT('Origin',(80.1322559480305,0.,0.));
#8317=CARTESIAN_POINT('',(85.8498933978656,-2.62112000702085,2.64359555743594));
#8318=CARTESIAN_POINT('',(85.6021262425917,-2.62112000711956,2.64359555733807));
#8319=CARTESIAN_POINT('',(80.1322559480305,-2.62112000711956,2.64359555733806));
#8320=CARTESIAN_POINT('Ctrl Pts',(85.8498933978656,-2.62112000692213,2.64359555753381));
#8321=CARTESIAN_POINT('Ctrl Pts',(85.8494125170131,-2.61469984289228,2.64996113805479));
#8322=CARTESIAN_POINT('Ctrl Pts',(85.848930638563,-2.60825646309207,2.65630335745762));
#8323=CARTESIAN_POINT('Ctrl Pts',(85.8458489244465,-2.56698787681799,2.69662909322084));
#8324=CARTESIAN_POINT('Ctrl Pts',(85.8432214558479,-2.53152355325839,2.72994934463062));
#8325=CARTESIAN_POINT('Ctrl Pts',(85.8359658805799,-2.43289520025543,2.81904010183764));
#8326=CARTESIAN_POINT('Ctrl Pts',(85.8312820259721,-2.36847745694498,2.87337417914566));
#8327=CARTESIAN_POINT('Ctrl Pts',(85.8114075654775,-2.09206654338741,3.0909027254847));
#8328=CARTESIAN_POINT('Ctrl Pts',(85.7955078393622,-1.86465625620216,3.23317943974336));
#8329=CARTESIAN_POINT('Ctrl Pts',(85.7714640352237,-1.49698235157898,3.41142758188823));
#8330=CARTESIAN_POINT('Ctrl Pts',(85.7632386578215,-1.36655037002493,3.46573806784839));
#8331=CARTESIAN_POINT('Ctrl Pts',(85.7531613681591,-1.19681762385791,3.52533594169434));
#8332=CARTESIAN_POINT('Ctrl Pts',(85.7510176185441,-1.16009569840774,3.53759015870344));
#8333=CARTESIAN_POINT('Ctrl Pts',(85.7475218576749,-1.09905520104518,3.55690679375909));
#8334=CARTESIAN_POINT('Ctrl Pts',(85.7461528219742,-1.07484430080951,3.56429770612739));
#8335=CARTESIAN_POINT('Ctrl Pts',(85.7432467446201,-1.02275182575708,3.57962098079737));
#8336=CARTESIAN_POINT('Ctrl Pts',(85.7417137672106,-0.994849938315332,3.58747562620802));
#8337=CARTESIAN_POINT('Ctrl Pts',(85.7372324883483,-0.91215881927862,3.6097149890045));
#8338=CARTESIAN_POINT('Ctrl Pts',(85.7343299480101,-0.857128003499739,3.62317653763189));
#8339=CARTESIAN_POINT('Ctrl Pts',(85.7274451946642,-0.72383229217003,3.65257587181262));
#8340=CARTESIAN_POINT('Ctrl Pts',(85.7235093567469,-0.645319034498762,3.66726166851202));
#8341=CARTESIAN_POINT('Ctrl Pts',(85.7121565910508,-0.414874513080685,3.702735200961));
#8342=CARTESIAN_POINT('Ctrl Pts',(85.7048734474978,-0.262059085519863,3.71667807391622));
#8343=CARTESIAN_POINT('Ctrl Pts',(85.6891413858099,0.0651469335017609,3.72624645831691));
#8344=CARTESIAN_POINT('Ctrl Pts',(85.6806827925711,0.239242970623695,3.71912800363517));
#8345=CARTESIAN_POINT('Ctrl Pts',(85.6684389236575,0.479841091312247,3.69232355566699));
#8346=CARTESIAN_POINT('Ctrl Pts',(85.6649480762204,0.547267475627297,3.68293338267451));
#8347=CARTESIAN_POINT('Ctrl Pts',(85.6592561784775,0.655002594250469,3.66490575877121));
#8348=CARTESIAN_POINT('Ctrl Pts',(85.657090943282,0.695492456425876,3.65743799486478));
#8349=CARTESIAN_POINT('Ctrl Pts',(85.6524853710776,0.78051783154468,3.64029338067007));
#8350=CARTESIAN_POINT('Ctrl Pts',(85.6500407449869,0.825015984046235,3.63046723746266));
#8351=CARTESIAN_POINT('Ctrl Pts',(85.6439332360755,0.934568833930955,3.60415752059903));
#8352=CARTESIAN_POINT('Ctrl Pts',(85.6402416538428,0.999377687447366,3.58672744926182));
#8353=CARTESIAN_POINT('Ctrl Pts',(85.6320561514306,1.13999146076088,3.54480303657727));
#8354=CARTESIAN_POINT('Ctrl Pts',(85.627543126425,1.2155518562535,3.51960816103044));
#8355=CARTESIAN_POINT('Ctrl Pts',(85.6126327662345,1.45916514393167,3.42959689751849));
#8356=CARTESIAN_POINT('Ctrl Pts',(85.6020007604734,1.62332641356021,3.35501140305426));
#8357=CARTESIAN_POINT('Ctrl Pts',(85.5814805775996,1.9285001938464,3.18869978857847));
#8358=CARTESIAN_POINT('Ctrl Pts',(85.5716190086118,2.06999904301061,3.09871431574759));
#8359=CARTESIAN_POINT('Ctrl Pts',(85.5595587943745,2.24207856363626,2.97221687858598));
#8360=CARTESIAN_POINT('Ctrl Pts',(85.5569896523303,2.27868544882367,2.94424565178728));
#8361=CARTESIAN_POINT('Ctrl Pts',(85.5529839106082,2.33585425333259,2.89885797228623));
#8362=CARTESIAN_POINT('Ctrl Pts',(85.551520386193,2.3567615918942,2.88188610521399));
#8363=CARTESIAN_POINT('Ctrl Pts',(85.548626061652,2.39819523930739,2.84749918324306));
#8364=CARTESIAN_POINT('Ctrl Pts',(85.5471953359125,2.41872051101255,2.8300853662804));
#8365=CARTESIAN_POINT('Ctrl Pts',(85.5433579601725,2.47381222978146,2.78230788623128));
#8366=CARTESIAN_POINT('Ctrl Pts',(85.5409791056765,2.50800849753616,2.75152282512411));
#8367=CARTESIAN_POINT('Ctrl Pts',(85.5306611561757,2.65588727662079,2.61334731541808));
#8368=CARTESIAN_POINT('Ctrl Pts',(85.5230790029957,2.76331656160075,2.49948204970793));
#8369=CARTESIAN_POINT('Ctrl Pts',(85.5022716823158,3.04002209971218,2.16647654460748));
#8370=CARTESIAN_POINT('Ctrl Pts',(85.4891887234473,3.19250624773465,1.93474797903165));
#8371=CARTESIAN_POINT('Ctrl Pts',(85.47187909144,3.34722883231301,1.63067569173227));
#8372=CARTESIAN_POINT('Ctrl Pts',(85.4685559607044,3.37503078443024,1.57232650732821));
#8373=CARTESIAN_POINT('Ctrl Pts',(85.4628483876903,3.41947367458326,1.47243552564367));
#8374=CARTESIAN_POINT('Ctrl Pts',(85.4604907503854,3.43691039258298,1.43126283925748));
#8375=CARTESIAN_POINT('Ctrl Pts',(85.4555942130232,3.47121720066883,1.34601092392358));
#8376=CARTESIAN_POINT('Ctrl Pts',(85.4530529585128,3.48799901786943,1.3019050804367));
#8377=CARTESIAN_POINT('Ctrl Pts',(85.4463380125565,3.52967032443349,1.18579024169859));
#8378=CARTESIAN_POINT('Ctrl Pts',(85.4421220719284,3.55319479678375,1.11331787986404));
#8379=CARTESIAN_POINT('Ctrl Pts',(85.4278154477226,3.62433610764735,0.868847195429822));
#8380=CARTESIAN_POINT('Ctrl Pts',(85.4174411252539,3.66180633316773,0.694169327647438));
#8381=CARTESIAN_POINT('Ctrl Pts',(85.392834817163,3.71988818380175,0.280396791140727));
#8382=CARTESIAN_POINT('Ctrl Pts',(85.3785385963413,3.73022116305746,0.0406324526124812));
#8383=CARTESIAN_POINT('Ctrl Pts',(85.3627570454361,3.71524903407227,-0.239802779125859));
#8384=CARTESIAN_POINT('Ctrl Pts',(85.3604583895618,3.71235311686573,-0.2810967342461));
#8385=CARTESIAN_POINT('Ctrl Pts',(85.3569101481204,3.70673782055373,-0.345705942664832));
#8386=CARTESIAN_POINT('Ctrl Pts',(85.3556376312755,3.70448572726458,-0.369057498967059));
#8387=CARTESIAN_POINT('Ctrl Pts',(85.3529187102068,3.69915127052956,-0.419385949559535));
#8388=CARTESIAN_POINT('Ctrl Pts',(85.3514764436293,3.6959942124392,-0.446353634928199));
#8389=CARTESIAN_POINT('Ctrl Pts',(85.3475682323122,3.6865454812577,-0.520072064656115));
#8390=CARTESIAN_POINT('Ctrl Pts',(85.3451318726982,3.67965970188688,-0.566742798567036));
#8391=CARTESIAN_POINT('Ctrl Pts',(85.3395916196952,3.66173418236234,-0.67406957710873));
#8392=CARTESIAN_POINT('Ctrl Pts',(85.3365129764802,3.65007103625863,-0.734608099702717));
#8393=CARTESIAN_POINT('Ctrl Pts',(85.3252800496085,3.60143289824589,-0.957161605531159));
#8394=CARTESIAN_POINT('Ctrl Pts',(85.3173762286619,3.55512653095226,-1.11694094788216));
#8395=CARTESIAN_POINT('Ctrl Pts',(85.3001054729591,3.43197222325973,-1.45535231424623));
#8396=CARTESIAN_POINT('Ctrl Pts',(85.2907327447734,3.35150841610452,-1.63213579751016));
#8397=CARTESIAN_POINT('Ctrl Pts',(85.2774557845002,3.22437572336044,-1.86198650195114));
#8398=CARTESIAN_POINT('Ctrl Pts',(85.2739322505664,3.18944771647931,-1.92120146302668));
#8399=CARTESIAN_POINT('Ctrl Pts',(85.2679636185365,3.12852335138933,-2.01824462694814));
#8400=CARTESIAN_POINT('Ctrl Pts',(85.2655506569088,3.10343033216894,-2.05662093359418));
#8401=CARTESIAN_POINT('Ctrl Pts',(85.2606475000304,3.05157019674382,-2.13282282073475));
#8402=CARTESIAN_POINT('Ctrl Pts',(85.2581571972093,3.02479292215194,-2.17063155993647));
#8403=CARTESIAN_POINT('Ctrl Pts',(85.2517598674181,2.95494613498814,-2.26545026047953));
#8404=CARTESIAN_POINT('Ctrl Pts',(85.2478178692362,2.91092957298447,-2.32173633867774));
#8405=CARTESIAN_POINT('Ctrl Pts',(85.2389523616222,2.80983480212235,-2.44361409664144));
#8406=CARTESIAN_POINT('Ctrl Pts',(85.2340036726254,2.75202409473727,-2.50854208009891));
#8407=CARTESIAN_POINT('Ctrl Pts',(85.2163467432131,2.54063045074661,-2.72985128265229));
#8408=CARTESIAN_POINT('Ctrl Pts',(85.2032930595409,2.37557168357753,-2.87463741791466));
#8409=CARTESIAN_POINT('Ctrl Pts',(85.1829314575854,2.0957060539676,-3.0794790603545));
#8410=CARTESIAN_POINT('Ctrl Pts',(85.1755199210211,1.98883749589948,-3.14955637642131));
#8411=CARTESIAN_POINT('Ctrl Pts',(85.1662368712596,1.84566411464876,-3.23324053975189));
#8412=CARTESIAN_POINT('Ctrl Pts',(85.1641273102985,1.81246198865685,-3.251968969095));
#8413=CARTESIAN_POINT('Ctrl Pts',(85.1606567965932,1.75660000656033,-3.28235782376432));
#8414=CARTESIAN_POINT('Ctrl Pts',(85.1592798801226,1.73409807999328,-3.29430120837918));
#8415=CARTESIAN_POINT('Ctrl Pts',(85.1563468197092,1.68539689389447,-3.31951308348748));
#8416=CARTESIAN_POINT('Ctrl Pts',(85.1547950039741,1.65916044506543,-3.33270408642881));
#8417=CARTESIAN_POINT('Ctrl Pts',(85.1501892710288,1.57999965504103,-3.37133750985229));
#8418=CARTESIAN_POINT('Ctrl Pts',(85.1471850461975,1.52662484611578,-3.39584051165289));
#8419=CARTESIAN_POINT('Ctrl Pts',(85.1399914619228,1.39539554547256,-3.45236465512013));
#8420=CARTESIAN_POINT('Ctrl Pts',(85.1358542780704,1.31699061623288,-3.48302848252433));
#8421=CARTESIAN_POINT('Ctrl Pts',(85.1160885191838,0.933256155186663,-3.61829266248534));
#8422=CARTESIAN_POINT('Ctrl Pts',(85.1010738685198,0.616260085628715,-3.68554414692541));
#8423=CARTESIAN_POINT('Ctrl Pts',(85.081350024612,0.227926993657657,-3.71636710174803));
#8424=CARTESIAN_POINT('Ctrl Pts',(85.077918962509,0.161169024941091,-3.71986007912614));
#8425=CARTESIAN_POINT('Ctrl Pts',(85.0720841124354,0.0492997851185086,-3.7226963920056));
#8426=CARTESIAN_POINT('Ctrl Pts',(85.0697102245506,0.00422829001023111,
-3.72302038483258));
#8427=CARTESIAN_POINT('Ctrl Pts',(85.0648293658586,-0.0874645238974345,
-3.72201449902313));
#8428=CARTESIAN_POINT('Ctrl Pts',(85.0623210719823,-0.134077060391818,-3.72062697016497));
#8429=CARTESIAN_POINT('Ctrl Pts',(85.0558113694728,-0.253683240855003,-3.71481612436998));
#8430=CARTESIAN_POINT('Ctrl Pts',(85.0517724667302,-0.326592447976102,-3.70911719869889));
#8431=CARTESIAN_POINT('Ctrl Pts',(85.0426394390116,-0.488565500018144,-3.69164399480658));
#8432=CARTESIAN_POINT('Ctrl Pts',(85.0375175152443,-0.577465003052578,-3.67878569470495));
#8433=CARTESIAN_POINT('Ctrl Pts',(85.0185665105707,-0.900075554077878,-3.62014172629223));
#8434=CARTESIAN_POINT('Ctrl Pts',(85.0043302629778,-1.1297127158424,-3.55517940493527));
#8435=CARTESIAN_POINT('Ctrl Pts',(84.9842332141465,-1.4503747442406,-3.43023749896758));
#8436=CARTESIAN_POINT('Ctrl Pts',(84.9781221854952,-1.54751443310165,-3.38752393648964));
#8437=CARTESIAN_POINT('Ctrl Pts',(84.9701580250113,-1.67545841412428,-3.32461110105688));
#8438=CARTESIAN_POINT('Ctrl Pts',(84.968141643808,-1.70797605986298,-3.30802325402185));
#8439=CARTESIAN_POINT('Ctrl Pts',(84.9647759067646,-1.76257341524357,-3.27915239787956));
#8440=CARTESIAN_POINT('Ctrl Pts',(84.9634127364409,-1.78478089016087,-3.26711842327509));
#8441=CARTESIAN_POINT('Ctrl Pts',(84.9604507297425,-1.83326785476274,-3.2402019091442));
#8442=CARTESIAN_POINT('Ctrl Pts',(84.9588574872331,-1.85949136645593,-3.22522424250651));
#8443=CARTESIAN_POINT('Ctrl Pts',(84.9539690640011,-1.94025208888828,-3.1777849298484));
#8444=CARTESIAN_POINT('Ctrl Pts',(84.9507330862616,-1.9941456363019,-3.14424541855897));
#8445=CARTESIAN_POINT('Ctrl Pts',(84.9428113759774,-2.12608845886024,-3.05737567525781));
#8446=CARTESIAN_POINT('Ctrl Pts',(84.9381929119439,-2.20301528826141,-3.00241959153895));
#8447=CARTESIAN_POINT('Ctrl Pts',(84.9185678173305,-2.52404053139152,-2.75409267142618));
#8448=CARTESIAN_POINT('Ctrl Pts',(84.9040006244252,-2.74542564463179,-2.5334644736033));
#8449=CARTESIAN_POINT('Ctrl Pts',(84.8849457241627,-2.97609980732259,-2.23736312836553));
#8450=CARTESIAN_POINT('Ctrl Pts',(84.8816530150491,-3.01412274848135,-2.18586991352904));
#8451=CARTESIAN_POINT('Ctrl Pts',(84.8759810676482,-3.07636478429085,-2.09686374878784));
#8452=CARTESIAN_POINT('Ctrl Pts',(84.8736277777281,-3.10127135509216,-2.05984796131509));
#8453=CARTESIAN_POINT('Ctrl Pts',(84.8687254047083,-3.15123777198564,-1.9826274510979));
#8454=CARTESIAN_POINT('Ctrl Pts',(84.8661736556554,-3.17620736358856,-1.94237422021055));
#8455=CARTESIAN_POINT('Ctrl Pts',(84.8593933479696,-3.23981416807579,-1.83532687415292));
#8456=CARTESIAN_POINT('Ctrl Pts',(84.8551209844165,-3.27715318897931,-1.76779138506349));
#8457=CARTESIAN_POINT('Ctrl Pts',(84.8406379902645,-3.39471293336672,-1.5386171887275));
#8458=CARTESIAN_POINT('Ctrl Pts',(84.8301386052237,-3.4652740466142,-1.37232769270576));
#8459=CARTESIAN_POINT('Ctrl Pts',(84.8056972840747,-3.59917856461861,-0.979672419790579));
#8460=CARTESIAN_POINT('Ctrl Pts',(84.7917089799957,-3.65372708853327,-0.751087971367));
#8461=CARTESIAN_POINT('Ctrl Pts',(84.7761637898157,-3.6922597031176,-0.477332705893551));
#8462=CARTESIAN_POINT('Ctrl Pts',(84.773832210272,-3.69740553180429,-0.435684348529494));
#8463=CARTESIAN_POINT('Ctrl Pts',(84.7702461400659,-3.70433890339234,-0.370534279777525));
#8464=CARTESIAN_POINT('Ctrl Pts',(84.7689679393714,-3.70660923130903,-0.347088510558622));
#8465=CARTESIAN_POINT('Ctrl Pts',(84.7662511585116,-3.71100372807919,-0.296728288935771));
#8466=CARTESIAN_POINT('Ctrl Pts',(84.764816477005,-3.71305798167571,-0.26980893158297));
#8467=CARTESIAN_POINT('Ctrl Pts',(84.7609547658138,-3.7178467677859,-0.196561671039895));
#8468=CARTESIAN_POINT('Ctrl Pts',(84.7585561428848,-3.72000825464481,-0.150199973066388));
#8469=CARTESIAN_POINT('Ctrl Pts',(84.7480399856682,-3.725762785653,0.0560879511793481));
#8470=CARTESIAN_POINT('Ctrl Pts',(84.7402953519644,-3.71991330361409,0.216118305932106));
#8471=CARTESIAN_POINT('Ctrl Pts',(84.7196210529788,-3.67652162113854,0.644360685837346));
#8472=CARTESIAN_POINT('Ctrl Pts',(84.706809428085,-3.62002126997029,0.909642036300186));
#8473=CARTESIAN_POINT('Ctrl Pts',(84.6897819242686,-3.51478315774588,1.22859606302154));
#8474=CARTESIAN_POINT('Ctrl Pts',(84.6864194839653,-3.4926473395465,1.29017938518824));
#8475=CARTESIAN_POINT('Ctrl Pts',(84.680665728801,-3.45262706651849,1.39292656799413));
#8476=CARTESIAN_POINT('Ctrl Pts',(84.678302336898,-3.43560009997883,1.43440921947389));
#8477=CARTESIAN_POINT('Ctrl Pts',(84.6734124454185,-3.39921069412584,1.51869697851222));
#8478=CARTESIAN_POINT('Ctrl Pts',(84.6708839801748,-3.37977900674372,1.56146324022775));
#8479=CARTESIAN_POINT('Ctrl Pts',(84.6642485205864,-3.3272339736198,1.67152804813198));
#8480=CARTESIAN_POINT('Ctrl Pts',(84.6601011402097,-3.29288799246592,1.73821158647624));
#8481=CARTESIAN_POINT('Ctrl Pts',(84.6443755031387,-3.15716404466941,1.9832442718456));
#8482=CARTESIAN_POINT('Ctrl Pts',(84.6323932353672,-3.04312485252166,2.15413962831931));
#8483=CARTESIAN_POINT('Ctrl Pts',(84.6115974044267,-2.82400503823443,2.43013714234308));
#8484=CARTESIAN_POINT('Ctrl Pts',(84.6028710314319,-2.72566535082345,2.5399390463136));
#8485=CARTESIAN_POINT('Ctrl Pts',(84.5943437838656,-2.62112000711956,2.64359555733806));
#8486=CARTESIAN_POINT('Ctrl Pts',(84.3497092098018,-2.62112000711955,2.64359555733807));
#8487=CARTESIAN_POINT('Ctrl Pts',(84.3577004554073,-2.71748852950729,2.5480463492204));
#8488=CARTESIAN_POINT('Ctrl Pts',(84.365757290069,-2.80864298662617,2.44721717317302));
#8489=CARTESIAN_POINT('Ctrl Pts',(84.378282986981,-2.94331207403744,2.2807655878376));
#8490=CARTESIAN_POINT('Ctrl Pts',(84.3828151482965,-2.99055360111133,2.21846069663541));
#8491=CARTESIAN_POINT('Ctrl Pts',(84.390442269409,-3.06808161814511,2.10923052520778));
#8492=CARTESIAN_POINT('Ctrl Pts',(84.393575905211,-3.09933847243202,2.06302687334104));
#8493=CARTESIAN_POINT('Ctrl Pts',(84.398236970433,-3.1451185658393,1.99196473508324));
#8494=CARTESIAN_POINT('Ctrl Pts',(84.3998068298419,-3.16041033343989,1.96761300259467));
#8495=CARTESIAN_POINT('Ctrl Pts',(84.4027208307145,-3.18858935888161,1.92156243169386));
#8496=CARTESIAN_POINT('Ctrl Pts',(84.4040685559681,-3.20154053814446,1.8999059123873));
#8497=CARTESIAN_POINT('Ctrl Pts',(84.4074519783387,-3.23381177980607,1.84467591264155));
#8498=CARTESIAN_POINT('Ctrl Pts',(84.4094700285399,-3.25283037852324,1.81092865817188));
#8499=CARTESIAN_POINT('Ctrl Pts',(84.4189161458612,-3.34047683614565,1.64956827490823));
#8500=CARTESIAN_POINT('Ctrl Pts',(84.4260088191148,-3.40214805511126,1.51830711116934));
#8501=CARTESIAN_POINT('Ctrl Pts',(84.4457737514687,-3.5543492488893,1.13818079816658));
#8502=CARTESIAN_POINT('Ctrl Pts',(84.4582131877736,-3.62622229714311,0.882815693192156));
#8503=CARTESIAN_POINT('Ctrl Pts',(84.4756120260174,-3.68439296953167,0.539544530916548));
#8504=CARTESIAN_POINT('Ctrl Pts',(84.4798574960193,-3.6955815612717,0.45665689540217));
#8505=CARTESIAN_POINT('Ctrl Pts',(84.4866918215267,-3.70882498821928,0.325311041065684));
#8506=CARTESIAN_POINT('Ctrl Pts',(84.4892245110254,-3.71274070412883,0.277067228053662));
#8507=CARTESIAN_POINT('Ctrl Pts',(84.4941341970363,-3.71844122889094,0.184475332889858));
#8508=CARTESIAN_POINT('Ctrl Pts',(84.49650620346,-3.72037573016654,0.140144642224046));
#8509=CARTESIAN_POINT('Ctrl Pts',(84.5021659787817,-3.72307235548542,0.0353799168115024));
#8510=CARTESIAN_POINT('Ctrl Pts',(84.5054736299707,-3.72315605913826,-0.0250576881961806));
#8511=CARTESIAN_POINT('Ctrl Pts',(84.5187103097967,-3.71767503342044,-0.2637322802509));
#8512=CARTESIAN_POINT('Ctrl Pts',(84.528966141924,-3.70077963699944,-0.441452222203766));
#8513=CARTESIAN_POINT('Ctrl Pts',(84.5539098353549,-3.63021470532582,-0.861144180428359));
#8514=CARTESIAN_POINT('Ctrl Pts',(84.5687358205277,-3.5650100027144,-1.100333979738));
#8515=CARTESIAN_POINT('Ctrl Pts',(84.5860047827334,-3.45657226886276,-1.38351087688137));
#8516=CARTESIAN_POINT('Ctrl Pts',(84.5891468768715,-3.43540104393102,-1.43527505765983));
#8517=CARTESIAN_POINT('Ctrl Pts',(84.5938171831602,-3.40158227314799,-1.51292211716394));
#8518=CARTESIAN_POINT('Ctrl Pts',(84.5953881106254,-3.38978813633711,-1.53916593948071));
#8519=CARTESIAN_POINT('Ctrl Pts',(84.5983022019282,-3.36708913967751,-1.58814798598555));
#8520=CARTESIAN_POINT('Ctrl Pts',(84.5996489929479,-3.35625566347617,-1.61091627222005));
#8521=CARTESIAN_POINT('Ctrl Pts',(84.6030266625163,-3.32823629904781,-1.66829364567193));
#8522=CARTESIAN_POINT('Ctrl Pts',(84.6050400146791,-3.31074092722445,-1.70274933222232));
#8523=CARTESIAN_POINT('Ctrl Pts',(84.6143352715038,-3.22644452121061,-1.86255089688336));
#8524=CARTESIAN_POINT('Ctrl Pts',(84.621295403141,-3.15303681970801,-1.98428966050968));
#8525=CARTESIAN_POINT('Ctrl Pts',(84.6410406995129,-2.9222678718785,-2.32171658785509));
#8526=CARTESIAN_POINT('Ctrl Pts',(84.6535726410647,-2.74847053307372,-2.52505946236985));
#8527=CARTESIAN_POINT('Ctrl Pts',(84.6711004456712,-2.49323323700584,-2.76581526337683));
#8528=CARTESIAN_POINT('Ctrl Pts',(84.6753707331877,-2.43009454097619,-2.82145091888547));
#8529=CARTESIAN_POINT('Ctrl Pts',(84.6822352590092,-2.32767955726113,-2.90570593456938));
#8530=CARTESIAN_POINT('Ctrl Pts',(84.684772419124,-2.28963388115275,-2.93577851796405));
#8531=CARTESIAN_POINT('Ctrl Pts',(84.689684803421,-2.21569575173613,-2.9919101005782));
#8532=CARTESIAN_POINT('Ctrl Pts',(84.6920548953846,-2.17990363250114,-3.01808774572552));
#8533=CARTESIAN_POINT('Ctrl Pts',(84.6977002575918,-2.09442789028804,-3.07828922433657));
#8534=CARTESIAN_POINT('Ctrl Pts',(84.7009951214694,-2.04437055131551,-3.11175854094892));
#8535=CARTESIAN_POINT('Ctrl Pts',(84.7138159689729,-1.84903673016673,-3.235614518653));
#8536=CARTESIAN_POINT('Ctrl Pts',(84.7236391931043,-1.69841974330997,-3.31715201385182));
#8537=CARTESIAN_POINT('Ctrl Pts',(84.7479920122739,-1.31973323863029,-3.48958709120933));
#8538=CARTESIAN_POINT('Ctrl Pts',(84.7626834021544,-1.08724328582523,-3.56886772400347));
#8539=CARTESIAN_POINT('Ctrl Pts',(84.7802662201671,-0.787989325480175,-3.63893141087296));
#8540=CARTESIAN_POINT('Ctrl Pts',(84.7837813380466,-0.72697828232875,-3.65160956315452));
#8541=CARTESIAN_POINT('Ctrl Pts',(84.788879245049,-0.636239233871519,-3.66810063443953));
#8542=CARTESIAN_POINT('Ctrl Pts',(84.7905164355045,-0.606739391609856,-3.67309543222682));
#8543=CARTESIAN_POINT('Ctrl Pts',(84.7934955622171,-0.552320147496168,-3.6816359587587));
#8544=CARTESIAN_POINT('Ctrl Pts',(84.7948424467651,-0.527421237112505,-3.68528529960259));
#8545=CARTESIAN_POINT('Ctrl Pts',(84.7981117805102,-0.466297767530757,-3.69361175474456));
#8546=CARTESIAN_POINT('Ctrl Pts',(84.8000197813375,-0.430038303987633,-3.69800874167732));
#8547=CARTESIAN_POINT('Ctrl Pts',(84.8074312458977,-0.2872274003076,-3.71319763317618));
#8548=CARTESIAN_POINT('Ctrl Pts',(84.8127561092886,-0.180289135961944,-3.71992409687582));
#8549=CARTESIAN_POINT('Ctrl Pts',(84.8295767722506,0.164010041812477,-3.72669558947464));
#8550=CARTESIAN_POINT('Ctrl Pts',(84.8407015703705,0.401127396292304,-3.70867385745816));
#8551=CARTESIAN_POINT('Ctrl Pts',(84.8566556212839,0.723208151667462,-3.65292561192162));
#8552=CARTESIAN_POINT('Ctrl Pts',(84.8610836372155,0.81091037342776,-3.63446264516046));
#8553=CARTESIAN_POINT('Ctrl Pts',(84.8692698506329,0.968644445172736,-3.59526295199708));
#8554=CARTESIAN_POINT('Ctrl Pts',(84.8729975277859,1.03889539064298,-3.57559551007754));
#8555=CARTESIAN_POINT('Ctrl Pts',(84.8792037271173,1.15286583215779,-3.54004601070367));
#8556=CARTESIAN_POINT('Ctrl Pts',(84.8816436983426,1.19694685735142,-3.52538556101324));
#8557=CARTESIAN_POINT('Ctrl Pts',(84.886490907348,1.28301329301346,-3.4949613325953));
#8558=CARTESIAN_POINT('Ctrl Pts',(84.8888959258565,1.32501107292667,-3.47925613432383));
#8559=CARTESIAN_POINT('Ctrl Pts',(84.8949203771632,1.42841816444954,-3.43844291032733));
#8560=CARTESIAN_POINT('Ctrl Pts',(84.8985681039725,1.48945768424577,-3.4124453331493));
#8561=CARTESIAN_POINT('Ctrl Pts',(84.9188714965433,1.82056840812455,-3.26084410961349));
#8562=CARTESIAN_POINT('Ctrl Pts',(84.9365427251537,2.07548164509976,-3.10481899919088));
#8563=CARTESIAN_POINT('Ctrl Pts',(84.9626552100353,2.42337840902794,-2.82972643773906));
#8564=CARTESIAN_POINT('Ctrl Pts',(84.9711577592578,2.53231637770362,-2.73267173304806));
#8565=CARTESIAN_POINT('Ctrl Pts',(84.9814765709189,2.66245344852988,-2.60224678598559));
#8566=CARTESIAN_POINT('Ctrl Pts',(84.9836061385242,2.68919595971497,-2.5746013323696));
#8567=CARTESIAN_POINT('Ctrl Pts',(84.9870947643311,2.73290653688442,-2.52799059985835));
#8568=CARTESIAN_POINT('Ctrl Pts',(84.98847033308,2.75011683155746,-2.50925729281321));
#8569=CARTESIAN_POINT('Ctrl Pts',(84.9913815536242,2.78651257298235,-2.46881638364625));
#8570=CARTESIAN_POINT('Ctrl Pts',(84.992913315754,2.80563886685551,-2.4470589100318));
#8571=CARTESIAN_POINT('Ctrl Pts',(84.9974099448455,2.86162074513969,-2.38185636680735));
#8572=CARTESIAN_POINT('Ctrl Pts',(85.0003283673633,2.89773643270886,-2.33778468658485));
#8573=CARTESIAN_POINT('Ctrl Pts',(85.014595141253,3.07200872301441,-2.11487448634548));
#8574=CARTESIAN_POINT('Ctrl Pts',(85.025263459563,3.19470160523901,-1.92453347120085));
#8575=CARTESIAN_POINT('Ctrl Pts',(85.0455503079162,3.39036456633071,-1.55012447362178));
#8576=CARTESIAN_POINT('Ctrl Pts',(85.0550920206195,3.46742023690693,-1.3691039040602));
#8577=CARTESIAN_POINT('Ctrl Pts',(85.0681982570292,3.54921537247631,-1.12501547196317));
#8578=CARTESIAN_POINT('Ctrl Pts',(85.0713445184174,3.56717440162158,-1.06670325151074));
#8579=CARTESIAN_POINT('Ctrl Pts',(85.0768611809925,3.59572773802157,-0.965186795515472));
#8580=CARTESIAN_POINT('Ctrl Pts',(85.0792099544731,3.60699580127323,-0.922184678932751));
#8581=CARTESIAN_POINT('Ctrl Pts',(85.0841548803673,3.62886513226993,-0.832181493252355));
#8582=CARTESIAN_POINT('Ctrl Pts',(85.0867548084219,3.63932934391094,-0.785155920977204));
#8583=CARTESIAN_POINT('Ctrl Pts',(85.0938763811283,3.66520401854062,-0.657214252047274));
#8584=CARTESIAN_POINT('Ctrl Pts',(85.0984506497198,3.67884578387839,-0.57597165853698));
#8585=CARTESIAN_POINT('Ctrl Pts',(85.1201971604326,3.73001510605877,-0.194046773395387));
#8586=CARTESIAN_POINT('Ctrl Pts',(85.1383329859209,3.73343268950547,0.110022995888035));
#8587=CARTESIAN_POINT('Ctrl Pts',(85.1606273071064,3.69135320513746,0.488760773943125));
#8588=CARTESIAN_POINT('Ctrl Pts',(85.1651588822328,3.68027876254556,0.566149168926117));
#8589=CARTESIAN_POINT('Ctrl Pts',(85.1727849575409,3.65714219045148,0.698060312522502));
#8590=CARTESIAN_POINT('Ctrl Pts',(85.1759181489983,3.64627508776562,0.752765440411813));
#8591=CARTESIAN_POINT('Ctrl Pts',(85.180578271632,3.6279499348975,0.835268241075232));
#8592=CARTESIAN_POINT('Ctrl Pts',(85.1821476462709,3.62139242573309,0.863255911161775));
#8593=CARTESIAN_POINT('Ctrl Pts',(85.1850608573952,3.6084722332037,0.915659388230615));
#8594=CARTESIAN_POINT('Ctrl Pts',(85.1864082764962,3.6021844974211,0.940090864992261));
#8595=CARTESIAN_POINT('Ctrl Pts',(85.189790465781,3.58561875875767,1.00185056647336));
#8596=CARTESIAN_POINT('Ctrl Pts',(85.1918076082838,3.5750056380014,1.03908678907127));
#8597=CARTESIAN_POINT('Ctrl Pts',(85.2012233817883,3.52209533629159,1.21430592386757));
#8598=CARTESIAN_POINT('Ctrl Pts',(85.2082893755242,3.47237567034827,1.34992905627698));
#8599=CARTESIAN_POINT('Ctrl Pts',(85.228050436351,3.30938647909909,1.72541323725623));
#8600=CARTESIAN_POINT('Ctrl Pts',(85.2405086361155,3.17822363890271,1.95652291091477));
#8601=CARTESIAN_POINT('Ctrl Pts',(85.2579339182321,2.97478963610414,2.23975556040008));
#8602=CARTESIAN_POINT('Ctrl Pts',(85.2621847287796,2.9236656896391,2.30609106965398));
#8603=CARTESIAN_POINT('Ctrl Pts',(85.2690256378613,2.83951645805101,2.40797808491458));
#8604=CARTESIAN_POINT('Ctrl Pts',(85.2715593779106,2.80795742860439,2.44470590665879));
#8605=CARTESIAN_POINT('Ctrl Pts',(85.276469873513,2.74612615890726,2.51388685394495));
#8606=CARTESIAN_POINT('Ctrl Pts',(85.2788416094157,2.71597228670018,2.54643482269269));
#8607=CARTESIAN_POINT('Ctrl Pts',(85.2844987398314,2.64341813425008,2.62199447093899));
#8608=CARTESIAN_POINT('Ctrl Pts',(85.2878039586191,2.60053958050775,2.66452767958982));
#8609=CARTESIAN_POINT('Ctrl Pts',(85.3009510727438,2.42817135095783,2.8273824941198));
#8610=CARTESIAN_POINT('Ctrl Pts',(85.3111132211399,2.29122817946343,2.93945049721122));
#8611=CARTESIAN_POINT('Ctrl Pts',(85.3355376890594,1.95067241343988,3.17984457878125));
#8612=CARTESIAN_POINT('Ctrl Pts',(85.3499237879498,1.74154920764749,3.2990214802251));
#8613=CARTESIAN_POINT('Ctrl Pts',(85.3671719110249,1.46627061835471,3.42238247810924));
#8614=CARTESIAN_POINT('Ctrl Pts',(85.3706408725114,1.40951888663837,3.44614402891544));
#8615=CARTESIAN_POINT('Ctrl Pts',(85.3756862618091,1.32445425507946,3.47930674326803));
#8616=CARTESIAN_POINT('Ctrl Pts',(85.3773155803586,1.29657728535777,3.4897911034479));
#8617=CARTESIAN_POINT('Ctrl Pts',(85.3802883933489,1.24488745391756,3.50852642723065));
#8618=CARTESIAN_POINT('Ctrl Pts',(85.3816366357756,1.2211131419708,3.51687150448457));
#8619=CARTESIAN_POINT('Ctrl Pts',(85.3849201194898,1.1624357002611,3.53680123612462));
#8620=CARTESIAN_POINT('Ctrl Pts',(85.3868405748137,1.1274426798099,3.54811117949107));
#8621=CARTESIAN_POINT('Ctrl Pts',(85.39432346002,0.988772230521879,3.59067147057664));
#8622=CARTESIAN_POINT('Ctrl Pts',(85.3997035933605,0.883913423917103,3.61791272603219));
#8623=CARTESIAN_POINT('Ctrl Pts',(85.4165070274933,0.547295124935531,3.68985036652612));
#8624=CARTESIAN_POINT('Ctrl Pts',(85.4275725426963,0.312415017983476,3.71711310825143));
#8625=CARTESIAN_POINT('Ctrl Pts',(85.4434538194815,-0.0128580484193436,
3.72380125251899));
#8626=CARTESIAN_POINT('Ctrl Pts',(85.4478728500395,-0.102279230451825,3.72241841526964));
#8627=CARTESIAN_POINT('Ctrl Pts',(85.4560444523055,-0.264292125795481,3.71407069718364));
#8628=CARTESIAN_POINT('Ctrl Pts',(85.4597666907731,-0.33689463674357,3.70818993688117));
#8629=CARTESIAN_POINT('Ctrl Pts',(85.4659662624008,-0.455424664730702,3.69507939925444));
#8630=CARTESIAN_POINT('Ctrl Pts',(85.4684052134145,-0.501473151472571,3.68911206375881));
#8631=CARTESIAN_POINT('Ctrl Pts',(85.4732521370592,-0.591757709752645,3.67569065115112));
#8632=CARTESIAN_POINT('Ctrl Pts',(85.4756579284664,-0.635994548465437,3.6682951965924));
#8633=CARTESIAN_POINT('Ctrl Pts',(85.4816878000442,-0.745387140320439,3.64796889681492));
#8634=CARTESIAN_POINT('Ctrl Pts',(85.4853402917949,-0.810349054877533,3.6340903555459));
#8635=CARTESIAN_POINT('Ctrl Pts',(85.5036193579078,-1.12900026294455,3.55704460246404));
#8636=CARTESIAN_POINT('Ctrl Pts',(85.5189999316127,-1.37589025717203,3.46902002242128));
#8637=CARTESIAN_POINT('Ctrl Pts',(85.544206758291,-1.76074837595394,3.28421194118139));
#8638=CARTESIAN_POINT('Ctrl Pts',(85.5539554571805,-1.90506893466202,3.20265547685798));
#8639=CARTESIAN_POINT('Ctrl Pts',(85.565967208129,-2.08271525574832,3.08599533683943));
#8640=CARTESIAN_POINT('Ctrl Pts',(85.5685867403336,-2.12145466387256,3.05949351324118));
#8641=CARTESIAN_POINT('Ctrl Pts',(85.5726477696777,-2.18169799228777,3.01658612822444));
#8642=CARTESIAN_POINT('Ctrl Pts',(85.5741175277645,-2.20354104537659,3.00066741721889));
#8643=CARTESIAN_POINT('Ctrl Pts',(85.5770000971864,-2.2465081159201,2.96863178157696));
#8644=CARTESIAN_POINT('Ctrl Pts',(85.5784132700148,-2.26763667848559,2.95252389157424));
#8645=CARTESIAN_POINT('Ctrl Pts',(85.5821639308893,-2.32380862651915,2.90874109603037));
#8646=CARTESIAN_POINT('Ctrl Pts',(85.5844755973894,-2.3585305341952,2.88065883903243));
#8647=CARTESIAN_POINT('Ctrl Pts',(85.5920223549565,-2.47176554424096,2.78565673760962));
#8648=CARTESIAN_POINT('Ctrl Pts',(85.5971138283267,-2.54795439720703,2.71613912151622));
#8649=CARTESIAN_POINT('Ctrl Pts',(85.6021262425917,-2.62112000711955,2.64359555733807));
#8650=CARTESIAN_POINT('Origin',(80.1322559480305,0.,0.));
#8651=CARTESIAN_POINT('',(87.0941439893651,-2.62112000711956,2.64359555733806));
#8652=CARTESIAN_POINT('',(86.8469367975355,-2.62112000721926,2.64359555723921));
#8653=CARTESIAN_POINT('',(80.1322559480305,-2.62112000711956,2.64359555733806));
#8654=CARTESIAN_POINT('Ctrl Pts',(87.0941439893651,-2.62112000711957,2.64359555733806));
#8655=CARTESIAN_POINT('Ctrl Pts',(87.0855458142099,-2.49744654314825,2.76621756351642));
#8656=CARTESIAN_POINT('Ctrl Pts',(87.0772681399053,-2.36524967169369,2.88008032166457));
#8657=CARTESIAN_POINT('Ctrl Pts',(87.0605578850035,-2.08604351812172,3.08829126272275));
#8658=CARTESIAN_POINT('Ctrl Pts',(87.0521479914016,-1.93950230334968,3.18236478723634));
#8659=CARTESIAN_POINT('Ctrl Pts',(87.0395835805447,-1.72012288643451,3.3023997723711));
#8660=CARTESIAN_POINT('Ctrl Pts',(87.0356995618198,-1.65221271376186,3.33689364085472));
#8661=CARTESIAN_POINT('Ctrl Pts',(87.0292966197469,-1.54059216483121,3.38934648306319));
#8662=CARTESIAN_POINT('Ctrl Pts',(87.0268211357132,-1.49751281774564,3.40859925751116));
#8663=CARTESIAN_POINT('Ctrl Pts',(87.0219464273946,-1.41291903643471,3.44449221701694));
#8664=CARTESIAN_POINT('Ctrl Pts',(87.0195503982968,-1.37144762996148,3.46121337138111));
#8665=CARTESIAN_POINT('Ctrl Pts',(87.0136303326449,-1.26930686870819,3.50027233558901));
#8666=CARTESIAN_POINT('Ctrl Pts',(87.0100805014871,-1.2083390665222,3.5217839726998));
#8667=CARTESIAN_POINT('Ctrl Pts',(86.9910935314529,-0.883827305684616,3.62686483882435));
#8668=CARTESIAN_POINT('Ctrl Pts',(86.9747910710472,-0.612172398951544,3.68245894365571));
#8669=CARTESIAN_POINT('Ctrl Pts',(86.9492481355891,-0.181110045307059,3.72163175568538));
#8670=CARTESIAN_POINT('Ctrl Pts',(86.9400597739562,-0.0245551509792661,
3.72595586967313));
#8671=CARTESIAN_POINT('Ctrl Pts',(86.9286263086855,0.177800686849849,3.71878632787191));
#8672=CARTESIAN_POINT('Ctrl Pts',(86.926060076226,0.223753597108814,3.71630455387948));
#8673=CARTESIAN_POINT('Ctrl Pts',(86.9220577646374,0.296496939635402,3.71102164552349));
#8674=CARTESIAN_POINT('Ctrl Pts',(86.9205948334473,0.323322155030927,3.70878079174956));
#8675=CARTESIAN_POINT('Ctrl Pts',(86.9177005830546,0.376927776711304,3.70371678215515));
#8676=CARTESIAN_POINT('Ctrl Pts',(86.9162693581982,0.403706589376467,3.70089362559444));
#8677=CARTESIAN_POINT('Ctrl Pts',(86.9124289256373,0.476200554206788,3.69245470844862));
#8678=CARTESIAN_POINT('Ctrl Pts',(86.9100475899422,0.52184709918323,3.68628060608361));
#8679=CARTESIAN_POINT('Ctrl Pts',(86.899175514567,0.732624250476652,3.65377721208441));
#8680=CARTESIAN_POINT('Ctrl Pts',(86.8910971414764,0.895988548172275,3.61718670001727));
#8681=CARTESIAN_POINT('Ctrl Pts',(86.8744182602416,1.22921093762203,3.51858006566514));
#8682=CARTESIAN_POINT('Ctrl Pts',(86.8658427885335,1.39812651832833,3.45493925542693));
#8683=CARTESIAN_POINT('Ctrl Pts',(86.8530708880048,1.63408538865602,3.34589008561808));
#8684=CARTESIAN_POINT('Ctrl Pts',(86.8491067696959,1.70531474899676,3.31015350233701));
#8685=CARTESIAN_POINT('Ctrl Pts',(86.8416761654682,1.83434276782321,3.24014818450169));
#8686=CARTESIAN_POINT('Ctrl Pts',(86.8382311025853,1.89246610934146,3.20654720497949));
#8687=CARTESIAN_POINT('Ctrl Pts',(86.8323560041769,1.98846977638627,3.14752796879192));
#8688=CARTESIAN_POINT('Ctrl Pts',(86.8299557942694,2.02684961967723,3.12295128777444));
#8689=CARTESIAN_POINT('Ctrl Pts',(86.8253386860813,2.09902248733288,3.07484420626856));
#8690=CARTESIAN_POINT('Ctrl Pts',(86.8231268162471,2.13289533227587,3.05144549593877));
#8691=CARTESIAN_POINT('Ctrl Pts',(86.8172040828554,2.22170691097764,2.987894860217));
#8692=CARTESIAN_POINT('Ctrl Pts',(86.8134583231719,2.27594290557852,2.94679153842116));
#8693=CARTESIAN_POINT('Ctrl Pts',(86.7999739708529,2.46436073570031,2.79569147128593));
#8694=CARTESIAN_POINT('Ctrl Pts',(86.7899487314597,2.59193573283884,2.67783923171364));
#8695=CARTESIAN_POINT('Ctrl Pts',(86.7690419502058,2.83593423743576,2.41860859997289));
#8696=CARTESIAN_POINT('Ctrl Pts',(86.7581711286196,2.95110229501105,2.2766612136569));
#8697=CARTESIAN_POINT('Ctrl Pts',(86.7438168938777,3.09221996613475,2.07393308105799));
#8698=CARTESIAN_POINT('Ctrl Pts',(86.7401076603712,3.12766820662185,2.02007797819577));
#8699=CARTESIAN_POINT('Ctrl Pts',(86.7337005448251,3.18741922823247,1.92395410053711));
#8700=CARTESIAN_POINT('Ctrl Pts',(86.7309776181362,3.21232367313618,1.88207804592705));
#8701=CARTESIAN_POINT('Ctrl Pts',(86.7267910275827,3.24997017146413,1.8158511716907));
#8702=CARTESIAN_POINT('Ctrl Pts',(86.7252964880628,3.26327615389606,1.79182879465593));
#8703=CARTESIAN_POINT('Ctrl Pts',(86.7223949737257,3.28887393801994,1.74438393210358));
#8704=CARTESIAN_POINT('Ctrl Pts',(86.7209870866751,3.30118415167598,1.72097365703609));
#8705=CARTESIAN_POINT('Ctrl Pts',(86.7172923381192,3.33314992697423,1.6585792244819));
#8706=CARTESIAN_POINT('Ctrl Pts',(86.7150297520048,3.35237159841283,1.61937594701949));
#8707=CARTESIAN_POINT('Ctrl Pts',(86.7016058151657,3.46380921807279,1.38160213446989));
#8708=CARTESIAN_POINT('Ctrl Pts',(86.6911928349078,3.5390588576568,1.17553355900645));
#8709=CARTESIAN_POINT('Ctrl Pts',(86.6712553906552,3.64680107102452,0.773662735985019));
#8710=CARTESIAN_POINT('Ctrl Pts',(86.6617749004971,3.682638297044,0.579551741808528));
#8711=CARTESIAN_POINT('Ctrl Pts',(86.6480995000784,3.71065098688795,0.309090854882502));
#8712=CARTESIAN_POINT('Ctrl Pts',(86.6442794901657,3.71611411609218,0.234441560619471));
#8713=CARTESIAN_POINT('Ctrl Pts',(86.637954043388,3.72133730444894,0.112782134637251));
#8714=CARTESIAN_POINT('Ctrl Pts',(86.6354899524438,3.72246350967918,0.0658506124230024));
#8715=CARTESIAN_POINT('Ctrl Pts',(86.6306181853865,3.72292984258869,-0.0259455538119476));
#8716=CARTESIAN_POINT('Ctrl Pts',(86.6282132695279,3.72234692770063,-0.0708018320245675));
#8717=CARTESIAN_POINT('Ctrl Pts',(86.6222334684651,3.71891762206235,-0.181151179838617));
#8718=CARTESIAN_POINT('Ctrl Pts',(86.6186315471276,3.71515172672389,-0.246598758624096));
#8719=CARTESIAN_POINT('Ctrl Pts',(86.5999624281649,3.68707407142453,-0.580536440304655));
#8720=CARTESIAN_POINT('Ctrl Pts',(86.5840822472199,3.63537925501826,-0.84588304490476));
#8721=CARTESIAN_POINT('Ctrl Pts',(86.5611812354376,3.52039994896723,-1.21642328869146));
#8722=CARTESIAN_POINT('Ctrl Pts',(86.5542092673796,3.47990959831581,-1.32783008563802));
#8723=CARTESIAN_POINT('Ctrl Pts',(86.5432894830621,3.40670773263547,-1.50275492081419));
#8724=CARTESIAN_POINT('Ctrl Pts',(86.5392488224445,3.37736341988888,-1.56759287309867));
#8725=CARTESIAN_POINT('Ctrl Pts',(86.5335063120669,3.33204517640462,-1.66053673718823));
#8726=CARTESIAN_POINT('Ctrl Pts',(86.5317340939855,3.31753676844222,-1.68933633279597));
#8727=CARTESIAN_POINT('Ctrl Pts',(86.5286256196694,3.29111200434737,-1.74013650741525));
#8728=CARTESIAN_POINT('Ctrl Pts',(86.5272812609262,3.27934546303361,-1.76221074074115));
#8729=CARTESIAN_POINT('Ctrl Pts',(86.524193199337,3.25152834733825,-1.81315241292133));
#8730=CARTESIAN_POINT('Ctrl Pts',(86.5224591029323,3.23531483432639,-1.84192734305363));
#8731=CARTESIAN_POINT('Ctrl Pts',(86.5164848776486,3.17748564426446,-1.94143955722141));
#8732=CARTESIAN_POINT('Ctrl Pts',(86.5123482894765,3.13391364560317,-2.01101702693795));
#8733=CARTESIAN_POINT('Ctrl Pts',(86.5011751645571,3.00785475746478,-2.19825142923168));
#8734=CARTESIAN_POINT('Ctrl Pts',(86.4942971452716,2.92080247638701,-2.31266427673389));
#8735=CARTESIAN_POINT('Ctrl Pts',(86.476657115048,2.68129050520715,-2.59228889376987));
#8736=CARTESIAN_POINT('Ctrl Pts',(86.4659001356468,2.52010626921958,-2.74924276152791));
#8737=CARTESIAN_POINT('Ctrl Pts',(86.4510622207759,2.29208630246345,-2.93427823933306));
#8738=CARTESIAN_POINT('Ctrl Pts',(86.4475189598073,2.23719533916555,-2.97634081802612));
#8739=CARTESIAN_POINT('Ctrl Pts',(86.4415267348762,2.14395401163627,-3.04375383942596));
#8740=CARTESIAN_POINT('Ctrl Pts',(86.4391104961513,2.10624754203616,-3.06996698458039));
#8741=CARTESIAN_POINT('Ctrl Pts',(86.4342085831539,2.02961037666456,-3.12116777702791));
#8742=CARTESIAN_POINT('Ctrl Pts',(86.4317229695238,1.99067965192145,-3.14614062603514));
#8743=CARTESIAN_POINT('Ctrl Pts',(86.4253550603507,1.89082744138003,-3.20759731251835));
#8744=CARTESIAN_POINT('Ctrl Pts',(86.4214384455877,1.82931065731527,-3.24307424058499));
#8745=CARTESIAN_POINT('Ctrl Pts',(86.4126426001675,1.6909784732218,-3.31766235986218));
#8746=CARTESIAN_POINT('Ctrl Pts',(86.4077388505561,1.6137443779867,-3.35590812804808));
#8747=CARTESIAN_POINT('Ctrl Pts',(86.3903949579205,1.3397470159581,-3.47994289762899));
#8748=CARTESIAN_POINT('Ctrl Pts',(86.3776233269253,1.13695734666717,-3.55137196653923));
#8749=CARTESIAN_POINT('Ctrl Pts',(86.3572043491199,0.800513779599716,-3.63808950096067));
#8750=CARTESIAN_POINT('Ctrl Pts',(86.3494805354369,0.670172311482159,-3.66434057082682));
#8751=CARTESIAN_POINT('Ctrl Pts',(86.3398764920265,0.500509054171064,-3.6891527259522));
#8752=CARTESIAN_POINT('Ctrl Pts',(86.3377392959107,0.462234053200812,-3.69414361669377));
#8753=CARTESIAN_POINT('Ctrl Pts',(86.3342510052988,0.398756464235332,-3.70141873879962));
#8754=CARTESIAN_POINT('Ctrl Pts',(86.3328830382304,0.373596380933726,-3.70404282859394));
#8755=CARTESIAN_POINT('Ctrl Pts',(86.3299755315039,0.319503941624645,-3.70912762325093));
#8756=CARTESIAN_POINT('Ctrl Pts',(86.3284401324259,0.290566378758705,-3.7115066724205));
#8757=CARTESIAN_POINT('Ctrl Pts',(86.3239429777239,0.204836103919728,-3.71754599313455));
#8758=CARTESIAN_POINT('Ctrl Pts',(86.321027476268,0.147982107180997,-3.72024299851896));
#8759=CARTESIAN_POINT('Ctrl Pts',(86.3141036958413,0.010717398369314,-3.72360251318449));
#8760=CARTESIAN_POINT('Ctrl Pts',(86.3101425053642,-0.0696974670677866,
-3.72296574440098));
#8761=CARTESIAN_POINT('Ctrl Pts',(86.2988048492034,-0.302427154719188,-3.71357879905024));
#8762=CARTESIAN_POINT('Ctrl Pts',(86.2915584193212,-0.454303501826466,-3.69807246864518));
#8763=CARTESIAN_POINT('Ctrl Pts',(86.2758715214262,-0.776365967934107,-3.64504530329007));
#8764=CARTESIAN_POINT('Ctrl Pts',(86.2674205407036,-0.945729228336533,-3.60481471541688));
#8765=CARTESIAN_POINT('Ctrl Pts',(86.2551853331724,-1.17660564015992,-3.53257679335916));
#8766=CARTESIAN_POINT('Ctrl Pts',(86.251694871993,-1.240987424411,-3.51047705085387));
#8767=CARTESIAN_POINT('Ctrl Pts',(86.2460034296643,-1.34328348412648,-3.47219699865792));
#8768=CARTESIAN_POINT('Ctrl Pts',(86.243838252034,-1.38159893956311,-3.45712983709102));
#8769=CARTESIAN_POINT('Ctrl Pts',(86.2392326614329,-1.46178118124307,-3.42405313610928));
#8770=CARTESIAN_POINT('Ctrl Pts',(86.2367879566774,-1.50358273210469,-3.40590411226489));
#8771=CARTESIAN_POINT('Ctrl Pts',(86.230679935572,-1.60609712198144,-3.35914027804693));
#8772=CARTESIAN_POINT('Ctrl Pts',(86.2269879089592,-1.66638761677131,-3.32964305925615));
#8773=CARTESIAN_POINT('Ctrl Pts',(86.2091932976294,-1.94901758955779,-3.18176654702833));
#8774=CARTESIAN_POINT('Ctrl Pts',(86.1944006840025,-2.15973722932481,-3.04266536129845));
#8775=CARTESIAN_POINT('Ctrl Pts',(86.169216171285,-2.49005394618175,-2.77290553420489));
#8776=CARTESIAN_POINT('Ctrl Pts',(86.1589138222307,-2.61739951071717,-2.65303619659709));
#8777=CARTESIAN_POINT('Ctrl Pts',(86.1464179422017,-2.76740547728743,-2.49048141597456));
#8778=CARTESIAN_POINT('Ctrl Pts',(86.1438229378442,-2.79830545385776,-2.45571124720149));
#8779=CARTESIAN_POINT('Ctrl Pts',(86.1397867243744,-2.84611253359111,-2.39984185863699));
#8780=CARTESIAN_POINT('Ctrl Pts',(86.1383179396979,-2.86345459783929,-2.37912281216687));
#8781=CARTESIAN_POINT('Ctrl Pts',(86.135422842045,-2.89756431081678,-2.33745766745448));
#8782=CARTESIAN_POINT('Ctrl Pts',(86.1339964309089,-2.91433411785479,-2.31651548893668));
#8783=CARTESIAN_POINT('Ctrl Pts',(86.1301855823582,-2.95897452684444,-2.25951631268135));
#8784=CARTESIAN_POINT('Ctrl Pts',(86.1278282771566,-2.98641260020816,-2.22312490629823));
#8785=CARTESIAN_POINT('Ctrl Pts',(86.1177217422589,-3.10277442550558,-2.06274948649478));
#8786=CARTESIAN_POINT('Ctrl Pts',(86.1103128245743,-3.18470336629118,-1.9338604285908));
#8787=CARTESIAN_POINT('Ctrl Pts',(86.0893523808962,-3.39548635608141,-1.55234841437216));
#8788=CARTESIAN_POINT('Ctrl Pts',(86.0759722848772,-3.50372002701962,-1.28959309939659));
#8789=CARTESIAN_POINT('Ctrl Pts',(86.0583532071486,-3.59851601870318,-0.95582858137754));
#8790=CARTESIAN_POINT('Ctrl Pts',(86.0550750166787,-3.61434444646365,-0.894113770380368));
#8791=CARTESIAN_POINT('Ctrl Pts',(86.049420014835,-3.6385418137654,-0.788585608670715));
#8792=CARTESIAN_POINT('Ctrl Pts',(86.0470687449336,-3.64772129451368,-0.744971761561947));
#8793=CARTESIAN_POINT('Ctrl Pts',(86.0421633000119,-3.66505384275882,-0.65459902877039));
#8794=CARTESIAN_POINT('Ctrl Pts',(86.03960630646,-3.6731000857277,-0.607828133473039));
#8795=CARTESIAN_POINT('Ctrl Pts',(86.0327933663423,-3.69194846270976,-0.484161597884745));
#8796=CARTESIAN_POINT('Ctrl Pts',(86.0284928312978,-3.70124232502587,-0.407062600228721));
#8797=CARTESIAN_POINT('Ctrl Pts',(86.0157266400444,-3.72134441612083,-0.180998079736236));
#8798=CARTESIAN_POINT('Ctrl Pts',(86.00708730696,-3.72560846721092,-0.0316144148200146));
#8799=CARTESIAN_POINT('Ctrl Pts',(85.9829417602206,-3.71260889016869,0.379658115342805));
#8800=CARTESIAN_POINT('Ctrl Pts',(85.9672084493833,-3.67666745044717,0.640100566253484));
#8801=CARTESIAN_POINT('Ctrl Pts',(85.9500084052455,-3.60326383863187,0.936605028838768));
#8802=CARTESIAN_POINT('Ctrl Pts',(85.9476014631639,-3.59213557664529,0.978417899278217));
#8803=CARTESIAN_POINT('Ctrl Pts',(85.9437865281443,-3.57305475768065,1.0453911774968));
#8804=CARTESIAN_POINT('Ctrl Pts',(85.942355579981,-3.56555942007055,1.07067696332788));
#8805=CARTESIAN_POINT('Ctrl Pts',(85.9394608085896,-3.54968239526689,1.12222193286415));
#8806=CARTESIAN_POINT('Ctrl Pts',(85.9379982970298,-3.5412766259267,1.1484716473878));
#8807=CARTESIAN_POINT('Ctrl Pts',(85.9339651033083,-3.5170479086983,1.22133726669736));
#8808=CARTESIAN_POINT('Ctrl Pts',(85.9314272721966,-3.50059031158341,1.26773759560353));
#8809=CARTESIAN_POINT('Ctrl Pts',(85.9256035099715,-3.46013458732882,1.37499597964378));
#8810=CARTESIAN_POINT('Ctrl Pts',(85.922346730334,-3.43544292963202,1.43557580391519));
#8811=CARTESIAN_POINT('Ctrl Pts',(85.9098687232766,-3.33347722772846,1.66802227806513));
#8812=CARTESIAN_POINT('Ctrl Pts',(85.9009550103049,-3.24479486307189,1.83457905393513));
#8813=CARTESIAN_POINT('Ctrl Pts',(85.8831081412568,-3.04614358579844,2.14783213426471));
#8814=CARTESIAN_POINT('Ctrl Pts',(85.8742064509636,-2.93721218060871,2.29454792517636));
#8815=CARTESIAN_POINT('Ctrl Pts',(85.8618214218512,-2.77832321480123,2.4786021816896));
#8816=CARTESIAN_POINT('Ctrl Pts',(85.8586911844676,-2.7375610733881,2.52355057492965));
#8817=CARTESIAN_POINT('Ctrl Pts',(85.8536571674366,-2.67121701921286,2.59320833759869));
#8818=CARTESIAN_POINT('Ctrl Pts',(85.8517829969788,-2.6463477451317,2.61858230270289));
#8819=CARTESIAN_POINT('Ctrl Pts',(85.8498933978656,-2.62112000692213,2.64359555753381));
#8820=CARTESIAN_POINT('Ctrl Pts',(85.6021262425917,-2.62112000711955,2.64359555733807));
#8821=CARTESIAN_POINT('Ctrl Pts',(85.6094336418923,-2.72778523837051,2.53783718181052));
#8822=CARTESIAN_POINT('Ctrl Pts',(85.6165766468792,-2.82802492016228,2.42564775805759));
#8823=CARTESIAN_POINT('Ctrl Pts',(85.631059435394,-3.01482777074672,2.18917000253605));
#8824=CARTESIAN_POINT('Ctrl Pts',(85.6383827669007,-3.10109853402161,2.0651478457525));
#8825=CARTESIAN_POINT('Ctrl Pts',(85.6499475555827,-3.22115097676676,1.86800332638407));
#8826=CARTESIAN_POINT('Ctrl Pts',(85.6540125321464,-3.2604934775963,1.7984524490018));
#8827=CARTESIAN_POINT('Ctrl Pts',(85.6606274941131,-3.31971414153624,1.685420721973));
#8828=CARTESIAN_POINT('Ctrl Pts',(85.663127751281,-3.34104607253202,1.64272817647168));
#8829=CARTESIAN_POINT('Ctrl Pts',(85.6680204254946,-3.38072824485395,1.55933831538893));
#8830=CARTESIAN_POINT('Ctrl Pts',(85.6704089298305,-3.39917880517853,1.51869768774041));
#8831=CARTESIAN_POINT('Ctrl Pts',(85.6761871584105,-3.4416012977448,1.42060633759097));
#8832=CARTESIAN_POINT('Ctrl Pts',(85.6795991351301,-3.46487106473743,1.36286820248788));
#8833=CARTESIAN_POINT('Ctrl Pts',(85.6993150376519,-3.58926161707752,1.03041519021633));
#8834=CARTESIAN_POINT('Ctrl Pts',(85.7166162947478,-3.65913445793586,0.745145018366971));
#8835=CARTESIAN_POINT('Ctrl Pts',(85.7425680414504,-3.71289027342828,0.308322627895861));
#8836=CARTESIAN_POINT('Ctrl Pts',(85.7512068635102,-3.72219052180465,0.16099850843398));
#8837=CARTESIAN_POINT('Ctrl Pts',(85.7620585756323,-3.72288832280654,-0.0313838469468115));
#8838=CARTESIAN_POINT('Ctrl Pts',(85.764559677511,-3.7222392938679,-0.0762718669992173));
#8839=CARTESIAN_POINT('Ctrl Pts',(85.7684811559764,-3.719912513768,-0.147738788510013));
#8840=CARTESIAN_POINT('Ctrl Pts',(85.7699268382657,-3.71876124636725,-0.174329434053604));
#8841=CARTESIAN_POINT('Ctrl Pts',(85.7728061260819,-3.71586915988495,-0.227841053166634));
#8842=CARTESIAN_POINT('Ctrl Pts',(85.774239283814,-3.71412070667581,-0.25475993083399));
#8843=CARTESIAN_POINT('Ctrl Pts',(85.7781128636817,-3.70854875306549,-0.328194805047213));
#8844=CARTESIAN_POINT('Ctrl Pts',(85.7805244048689,-3.70414278585925,-0.374662886594448));
#8845=CARTESIAN_POINT('Ctrl Pts',(85.7919118354511,-3.67886027487737,-0.596772586514175));
#8846=CARTESIAN_POINT('Ctrl Pts',(85.8004266269106,-3.64635636776082,-0.77087340925476));
#8847=CARTESIAN_POINT('Ctrl Pts',(85.8202265783356,-3.54187050008689,-1.1703530285236));
#8848=CARTESIAN_POINT('Ctrl Pts',(85.8314676291454,-3.46057341830572,-1.39247852813938));
#8849=CARTESIAN_POINT('Ctrl Pts',(85.8470483893948,-3.32711278545684,-1.67170178882832));
#8850=CARTESIAN_POINT('Ctrl Pts',(85.8508021503739,-3.29347234355921,-1.73703926029697));
#8851=CARTESIAN_POINT('Ctrl Pts',(85.8570397865017,-3.23539841569795,-1.84207259083393));
#8852=CARTESIAN_POINT('Ctrl Pts',(85.859484281786,-3.21211345711308,-1.88238179540526));
#8853=CARTESIAN_POINT('Ctrl Pts',(85.8643318984126,-3.16496500330118,-1.960578486863));
#8854=CARTESIAN_POINT('Ctrl Pts',(85.8667326135437,-3.14116167662022,-1.99849307303521));
#8855=CARTESIAN_POINT('Ctrl Pts',(85.8727291437289,-3.08063142688979,-2.09115340586547));
#8856=CARTESIAN_POINT('Ctrl Pts',(85.8763526716693,-3.04312407427268,-2.14536889191235));
#8857=CARTESIAN_POINT('Ctrl Pts',(85.8948305632577,-2.84732189912131,-2.41292093141666));
#8858=CARTESIAN_POINT('Ctrl Pts',(85.9104691885054,-2.6679702717156,-2.60985217437065));
#8859=CARTESIAN_POINT('Ctrl Pts',(85.9332557825219,-2.3791123891087,-2.86586661738805));
#8860=CARTESIAN_POINT('Ctrl Pts',(85.9403461461548,-2.2851721077665,-2.94131906360297));
#8861=CARTESIAN_POINT('Ctrl Pts',(85.9502774370432,-2.1456865749998,-3.04263007028026));
#8862=CARTESIAN_POINT('Ctrl Pts',(85.9532414755997,-2.10299942242138,-3.07228945197199));
#8863=CARTESIAN_POINT('Ctrl Pts',(85.9585019421841,-2.02504584653918,-3.12406593159353));
#8864=CARTESIAN_POINT('Ctrl Pts',(85.9608132193774,-1.99000313488291,-3.14650384279586));
#8865=CARTESIAN_POINT('Ctrl Pts',(85.9645119501369,-1.93248120565692,-3.18198975367186));
#8866=CARTESIAN_POINT('Ctrl Pts',(85.9659201486685,-1.91022903451263,-3.19539787347497));
#8867=CARTESIAN_POINT('Ctrl Pts',(85.9688053762752,-1.86385742251669,-3.2226816725322));
#8868=CARTESIAN_POINT('Ctrl Pts',(85.9702804018078,-1.83971955252277,-3.23652185477435));
#8869=CARTESIAN_POINT('Ctrl Pts',(85.9744133253612,-1.7709565529244,-3.27493133210099));
#8870=CARTESIAN_POINT('Ctrl Pts',(85.9770354763526,-1.7259778334231,-3.2988578828701));
#8871=CARTESIAN_POINT('Ctrl Pts',(85.9913962102537,-1.47328754320206,-3.42669343696744));
#8872=CARTESIAN_POINT('Ctrl Pts',(86.0023611623734,-1.25668145724071,-3.51191889495602));
#8873=CARTESIAN_POINT('Ctrl Pts',(86.0224058116583,-0.855528912435574,-3.62784625069497));
#8874=CARTESIAN_POINT('Ctrl Pts',(86.0313873383303,-0.67394581621557,-3.66592250707809));
#8875=CARTESIAN_POINT('Ctrl Pts',(86.0441784881778,-0.423336707274367,-3.69921830298302));
#8876=CARTESIAN_POINT('Ctrl Pts',(86.0476436447068,-0.356152264758712,-3.70628990756546));
#8877=CARTESIAN_POINT('Ctrl Pts',(86.0535345720127,-0.243460576768844,-3.71505908397342));
#8878=CARTESIAN_POINT('Ctrl Pts',(86.0559297652706,-0.198046579904935,-3.71775663057157));
#8879=CARTESIAN_POINT('Ctrl Pts',(86.0605245883197,-0.111771546996656,-3.72129602543825));
#8880=CARTESIAN_POINT('Ctrl Pts',(86.062718975586,-0.0709236341024881,-3.72229857049041));
#8881=CARTESIAN_POINT('Ctrl Pts',(86.0685621080425,0.0368633114303421,-3.72316919094131));
#8882=CARTESIAN_POINT('Ctrl Pts',(86.0722442827751,0.103794409393507,-3.72190457606413));
#8883=CARTESIAN_POINT('Ctrl Pts',(86.0941793525446,0.496607901386395,-3.7038789046566));
#8884=CARTESIAN_POINT('Ctrl Pts',(86.1136801770067,0.819152171839487,-3.64613029422204));
#8885=CARTESIAN_POINT('Ctrl Pts',(86.1375922385336,1.2080275068535,-3.52225056611702));
#8886=CARTESIAN_POINT('Ctrl Pts',(86.1423511341087,1.28525028754994,-3.4948122104607));
#8887=CARTESIAN_POINT('Ctrl Pts',(86.1503077796218,1.41512175976555,-3.44377935810376));
#8888=CARTESIAN_POINT('Ctrl Pts',(86.1535483492848,1.46824235355526,-3.42146911900172));
#8889=CARTESIAN_POINT('Ctrl Pts',(86.1583322558526,1.54737228766557,-3.38605263095209));
#8890=CARTESIAN_POINT('Ctrl Pts',(86.1599212756287,1.57377897847635,-3.37386028920838));
#8891=CARTESIAN_POINT('Ctrl Pts',(86.1628637434502,1.62297218004048,-3.3504438299677));
#8892=CARTESIAN_POINT('Ctrl Pts',(86.1642209587629,1.64579089228138,-3.33929407351586));
#8893=CARTESIAN_POINT('Ctrl Pts',(86.1675859750896,1.70263623960033,-3.31079387499808));
#8894=CARTESIAN_POINT('Ctrl Pts',(86.1695771275474,1.7365140551866,-3.29315128736327));
#8895=CARTESIAN_POINT('Ctrl Pts',(86.1782735935378,1.88512324673912,-3.21282876333205));
#8896=CARTESIAN_POINT('Ctrl Pts',(86.1847083241853,1.99678613245855,-3.14464763955368));
#8897=CARTESIAN_POINT('Ctrl Pts',(86.2015442129889,2.28344904665274,-2.94817254448311));
#8898=CARTESIAN_POINT('Ctrl Pts',(86.2117574812673,2.45121262745509,-2.81023468303297));
#8899=CARTESIAN_POINT('Ctrl Pts',(86.2265866333393,2.66775178280323,-2.59796852548684));
#8900=CARTESIAN_POINT('Ctrl Pts',(86.2308674078235,2.7273536437863,-2.53532661106948));
#8901=CARTESIAN_POINT('Ctrl Pts',(86.2388140401587,2.83190804503613,-2.41748217291102));
#8902=CARTESIAN_POINT('Ctrl Pts',(86.2424523992356,2.87756139807176,-2.36295637280083));
#8903=CARTESIAN_POINT('Ctrl Pts',(86.2485508544632,2.95020599584887,-2.27096436095651));
#8904=CARTESIAN_POINT('Ctrl Pts',(86.2509751781328,2.97811225675103,-2.23424297828305));
#8905=CARTESIAN_POINT('Ctrl Pts',(86.2558502219406,3.03225768743813,-2.16017662162868));
#8906=CARTESIAN_POINT('Ctrl Pts',(86.2582999697757,3.05850661325295,-2.12284873900441));
#8907=CARTESIAN_POINT('Ctrl Pts',(86.2644827682683,3.1223423238136,-2.02842731126995));
#8908=CARTESIAN_POINT('Ctrl Pts',(86.2682464472412,3.1590541912884,-1.97076501299057));
#8909=CARTESIAN_POINT('Ctrl Pts',(86.2822501270715,3.28784219863828,-1.75562815569611));
#8910=CARTESIAN_POINT('Ctrl Pts',(86.2928126484244,3.36988997447111,-1.59247156208578));
#8911=CARTESIAN_POINT('Ctrl Pts',(86.3170740741648,3.52769265559509,-1.21129572531365));
#8912=CARTESIAN_POINT('Ctrl Pts',(86.330827827552,3.59582661525552,-0.990903577231676));
#8913=CARTESIAN_POINT('Ctrl Pts',(86.3469111478564,3.65404661263854,-0.713868381899681));
#8914=CARTESIAN_POINT('Ctrl Pts',(86.3498767838918,3.66382000005905,-0.661882362797964));
#8915=CARTESIAN_POINT('Ctrl Pts',(86.3543427455874,3.67710126324904,-0.58188409825047));
#8916=CARTESIAN_POINT('Ctrl Pts',(86.3558806472766,3.68140369666507,-0.554012387597388));
#8917=CARTESIAN_POINT('Ctrl Pts',(86.3587906965812,3.68903056385189,-0.500584685683449));
#8918=CARTESIAN_POINT('Ctrl Pts',(86.3601652289537,3.69240705149697,-0.475038645460873));
#8919=CARTESIAN_POINT('Ctrl Pts',(86.3636623313721,3.70040048840102,-0.409315460613231));
#8920=CARTESIAN_POINT('Ctrl Pts',(86.3657651577478,3.70462863856448,-0.369093247543778));
#8921=CARTESIAN_POINT('Ctrl Pts',(86.3774551740364,3.72474632319961,-0.142212282328467));
#8922=CARTESIAN_POINT('Ctrl Pts',(86.3864782020954,3.72718561104498,0.0453848181484849));
#8923=CARTESIAN_POINT('Ctrl Pts',(86.4074123558229,3.69993653230495,0.481062296494694));
#8924=CARTESIAN_POINT('Ctrl Pts',(86.4192745286475,3.65945858145486,0.727533263752532));
#8925=CARTESIAN_POINT('Ctrl Pts',(86.4353032379562,3.57706323554412,1.03347413285861));
#8926=CARTESIAN_POINT('Ctrl Pts',(86.4387756551994,3.55768013100455,1.09834491365597));
#8927=CARTESIAN_POINT('Ctrl Pts',(86.4444386148511,3.52374258830148,1.20157597714243));
#8928=CARTESIAN_POINT('Ctrl Pts',(86.4465937620554,3.51030368249267,1.24028808776818));
#8929=CARTESIAN_POINT('Ctrl Pts',(86.4511780388182,3.48064771360083,1.32136919929824));
#8930=CARTESIAN_POINT('Ctrl Pts',(86.4536114262528,3.46428980163189,1.36367921236376));
#8931=CARTESIAN_POINT('Ctrl Pts',(86.4596894967195,3.42194913328693,1.46751176925353));
#8932=CARTESIAN_POINT('Ctrl Pts',(86.4633625899263,3.39507696853425,1.52865243643085));
#8933=CARTESIAN_POINT('Ctrl Pts',(86.4771067756071,3.28989239037969,1.75149959088456));
#8934=CARTESIAN_POINT('Ctrl Pts',(86.4874932118722,3.20155688499758,1.90818348412831));
#8935=CARTESIAN_POINT('Ctrl Pts',(86.5127059823591,2.96436471724337,2.26575471392178));
#8936=CARTESIAN_POINT('Ctrl Pts',(86.5276458020231,2.80591308779361,2.45926046121373));
#8937=CARTESIAN_POINT('Ctrl Pts',(86.5442816273993,2.59721298358559,2.66747180694048));
#8938=CARTESIAN_POINT('Ctrl Pts',(86.5468075871259,2.56454887025487,2.69889061886849));
#8939=CARTESIAN_POINT('Ctrl Pts',(86.5507583584423,2.51173992788472,2.74786153182594));
#8940=CARTESIAN_POINT('Ctrl Pts',(86.5522090861148,2.49196660515143,2.76580603000567));
#8941=CARTESIAN_POINT('Ctrl Pts',(86.5550886980006,2.45190159524077,2.80138693408787));
#8942=CARTESIAN_POINT('Ctrl Pts',(86.5565173153271,2.43160854413421,2.81901936172574));
#8943=CARTESIAN_POINT('Ctrl Pts',(86.5603630523863,2.3759150417036,2.86636196805136));
#8944=CARTESIAN_POINT('Ctrl Pts',(86.562751992318,2.34014861075166,2.8956360371964));
#8945=CARTESIAN_POINT('Ctrl Pts',(86.5732100843242,2.17896634044315,3.02262261702539));
#8946=CARTESIAN_POINT('Ctrl Pts',(86.5809104931853,2.04790355723857,3.11291513339007));
#8947=CARTESIAN_POINT('Ctrl Pts',(86.6016278425068,1.67782827902271,3.33434938986421));
#8948=CARTESIAN_POINT('Ctrl Pts',(86.6145200852957,1.4295853158366,3.44808209823842));
#8949=CARTESIAN_POINT('Ctrl Pts',(86.6316253027507,1.10939474106273,3.55420110107961));
#8950=CARTESIAN_POINT('Ctrl Pts',(86.6349699444393,1.04710146829464,3.57304912306805));
#8951=CARTESIAN_POINT('Ctrl Pts',(86.6406945523442,0.941309170392913,3.60205444601581));
#8952=CARTESIAN_POINT('Ctrl Pts',(86.6430469381703,0.898062482272044,3.61307939838748));
#8953=CARTESIAN_POINT('Ctrl Pts',(86.6479142931884,0.809119127503158,3.63405836451464));
#8954=CARTESIAN_POINT('Ctrl Pts',(86.650431221566,0.763412311686202,3.64393404641464));
#8955=CARTESIAN_POINT('Ctrl Pts',(86.6570346075175,0.644302817319845,3.6673302281978));
#8956=CARTESIAN_POINT('Ctrl Pts',(86.6611610442062,0.570660559141779,3.67950847044678));
#8957=CARTESIAN_POINT('Ctrl Pts',(86.6754693191187,0.318019203136027,3.71352107942811));
#8958=CARTESIAN_POINT('Ctrl Pts',(86.6859467858589,0.137838618860974,3.72456226785177));
#8959=CARTESIAN_POINT('Ctrl Pts',(86.7107371972345,-0.28313509616538,3.71976547674153));
#8960=CARTESIAN_POINT('Ctrl Pts',(86.7251150891141,-0.523029518351199,3.69367991143006));
#8961=CARTESIAN_POINT('Ctrl Pts',(86.7409546000593,-0.799030907163151,3.63622214874936));
#8962=CARTESIAN_POINT('Ctrl Pts',(86.7432402383791,-0.839189095120821,3.62716471148247));
#8963=CARTESIAN_POINT('Ctrl Pts',(86.7467696285501,-0.90187715937815,3.61192888146062));
#8964=CARTESIAN_POINT('Ctrl Pts',(86.7480360551279,-0.924512311830358,3.60620156278309));
#8965=CARTESIAN_POINT('Ctrl Pts',(86.7507417433643,-0.973218841064589,3.59338871458555));
#8966=CARTESIAN_POINT('Ctrl Pts',(86.7521769135995,-0.99927006793809,3.58623155772152));
#8967=CARTESIAN_POINT('Ctrl Pts',(86.7560628418112,-1.07030241605493,3.56588241436927));
#8968=CARTESIAN_POINT('Ctrl Pts',(86.7584844057759,-1.11511711927446,3.55212314570359));
#8969=CARTESIAN_POINT('Ctrl Pts',(86.7692768214476,-1.31648417581484,3.48611146000874));
#8970=CARTESIAN_POINT('Ctrl Pts',(86.7772513941482,-1.46972730278891,3.42432677312787));
#8971=CARTESIAN_POINT('Ctrl Pts',(86.7977626258426,-1.8545619878887,3.23855701052766));
#8972=CARTESIAN_POINT('Ctrl Pts',(86.8102101350408,-2.07802282709313,3.09991344118273));
#8973=CARTESIAN_POINT('Ctrl Pts',(86.8268524963812,-2.33741100034856,2.89823658910978));
#8974=CARTESIAN_POINT('Ctrl Pts',(86.8302577577166,-2.38866603906616,2.8561406466196));
#8975=CARTESIAN_POINT('Ctrl Pts',(86.8360539529182,-2.47263967099234,2.7833308232452));
#8976=CARTESIAN_POINT('Ctrl Pts',(86.8384155708165,-2.5059774204876,2.75335329266576));
#8977=CARTESIAN_POINT('Ctrl Pts',(86.8428292837073,-2.56662102961766,2.69680823427543));
#8978=CARTESIAN_POINT('Ctrl Pts',(86.8448742045467,-2.59407595105526,2.67040968790267));
#8979=CARTESIAN_POINT('Ctrl Pts',(86.8469367975355,-2.62112000731897,2.64359555714035));
#8980=CARTESIAN_POINT('Origin',(80.1322559480305,0.,0.));
#8981=CARTESIAN_POINT('',(88.3477258685014,-2.62111999776108,2.64359556661698));
#8982=CARTESIAN_POINT('',(88.102942454071,-2.6211200160691,2.64359554846461));
#8983=CARTESIAN_POINT('',(80.1322559480305,-2.62112000711956,2.64359555733806));
#8984=CARTESIAN_POINT('Ctrl Pts',(88.3477258692703,-2.62111999772913,2.64359556664866));
#8985=CARTESIAN_POINT('Ctrl Pts',(88.346587856507,-2.60731572712132,2.65728247481293));
#8986=CARTESIAN_POINT('Ctrl Pts',(88.3454476547785,-2.59340290379044,2.67086259508366));
#8987=CARTESIAN_POINT('Ctrl Pts',(88.3352752980427,-2.46852116444019,2.79086171869281));
#8988=CARTESIAN_POINT('Ctrl Pts',(88.3261407576867,-2.35116788088766,2.8904178255313));
#8989=CARTESIAN_POINT('Ctrl Pts',(88.3124828443607,-2.16425177741569,3.03005159902215));
#8990=CARTESIAN_POINT('Ctrl Pts',(88.307866055008,-2.0989946068456,3.07561720664413));
#8991=CARTESIAN_POINT('Ctrl Pts',(88.3001131433989,-1.9849836243823,3.14990480204794));
#8992=CARTESIAN_POINT('Ctrl Pts',(88.2969368685854,-1.93694395398754,3.17967121184207));
#8993=CARTESIAN_POINT('Ctrl Pts',(88.2922229086738,-1.86328757730245,3.22302116889539));
#8994=CARTESIAN_POINT('Ctrl Pts',(88.2906415544796,-1.83816087605693,3.23741729646948));
#8995=CARTESIAN_POINT('Ctrl Pts',(88.2877114230548,-1.79075337008403,3.26384910984428));
#8996=CARTESIAN_POINT('Ctrl Pts',(88.2863589147069,-1.76851376001106,3.27595295141795));
#8997=CARTESIAN_POINT('Ctrl Pts',(88.282969248976,-1.71192040711382,3.3060094374264));
#8998=CARTESIAN_POINT('Ctrl Pts',(88.2809496976411,-1.67740573065636,3.32365463346486));
#8999=CARTESIAN_POINT('Ctrl Pts',(88.2716171754733,-1.51461038919857,3.40369962527841));
#9000=CARTESIAN_POINT('Ctrl Pts',(88.264628658243,-1.3830773880799,3.45923681301132));
#9001=CARTESIAN_POINT('Ctrl Pts',(88.2448762116589,-0.997765129077215,3.59642419566466));
#9002=CARTESIAN_POINT('Ctrl Pts',(88.2323609131233,-0.738007829348195,3.65857139934818));
#9003=CARTESIAN_POINT('Ctrl Pts',(88.2148579950487,-0.39052967315798,3.70316208239336));
#9004=CARTESIAN_POINT('Ctrl Pts',(88.210594226684,-0.306883504553843,3.7110300557328));
#9005=CARTESIAN_POINT('Ctrl Pts',(88.2037301592572,-0.174522952423965,3.7189746302174));
#9006=CARTESIAN_POINT('Ctrl Pts',(88.2011865391862,-0.12594877912364,3.72093633119087));
#9007=CARTESIAN_POINT('Ctrl Pts',(88.1962544367835,-0.0327782771470576,
3.72287265153038));
#9008=CARTESIAN_POINT('Ctrl Pts',(88.1938709705507,0.0118066390679314,3.72299819609961));
#9009=CARTESIAN_POINT('Ctrl Pts',(88.1881803952586,0.117154107394293,3.72140250392247));
#9010=CARTESIAN_POINT('Ctrl Pts',(88.1848531310075,0.177892132621967,3.71899388089514));
#9011=CARTESIAN_POINT('Ctrl Pts',(88.1710246036501,0.426733978994542,3.70301607101617));
#9012=CARTESIAN_POINT('Ctrl Pts',(88.1601521792555,0.613714655913062,3.67665197761381));
#9013=CARTESIAN_POINT('Ctrl Pts',(88.1341127710137,1.04689980084175,3.58160124693435));
#9014=CARTESIAN_POINT('Ctrl Pts',(88.1188294509274,1.28965654346071,3.50152250269973));
#9015=CARTESIAN_POINT('Ctrl Pts',(88.1018992440904,1.56350875938017,3.37880812117282));
#9016=CARTESIAN_POINT('Ctrl Pts',(88.0993844281695,1.60435261156045,3.35960667518108));
#9017=CARTESIAN_POINT('Ctrl Pts',(88.0954427303683,1.66882526709724,3.32785286592769));
#9018=CARTESIAN_POINT('Ctrl Pts',(88.0939902673595,1.69268449029694,3.31578072058256));
#9019=CARTESIAN_POINT('Ctrl Pts',(88.0910968820672,1.74047197227789,3.29095123199137));
#9020=CARTESIAN_POINT('Ctrl Pts',(88.0896564256769,1.76439497419444,3.27818748109516));
#9021=CARTESIAN_POINT('Ctrl Pts',(88.0857594842002,1.82938598120682,3.24259494668789));
#9022=CARTESIAN_POINT('Ctrl Pts',(88.0833322943385,1.87016571719005,3.21924768018041));
#9023=CARTESIAN_POINT('Ctrl Pts',(88.068884183962,2.11366607786852,3.07364937988587));
#9024=CARTESIAN_POINT('Ctrl Pts',(88.0577067526452,2.30480616356035,2.93305199732271));
#9025=CARTESIAN_POINT('Ctrl Pts',(88.0373616804602,2.62083602712351,2.65049345396393));
#9026=CARTESIAN_POINT('Ctrl Pts',(88.0282955238868,2.75074743596031,2.51540814458643));
#9027=CARTESIAN_POINT('Ctrl Pts',(88.0153933280264,2.91321046399893,2.31876837962986));
#9028=CARTESIAN_POINT('Ctrl Pts',(88.011909171481,2.95503370283284,2.26522782595828));
#9029=CARTESIAN_POINT('Ctrl Pts',(88.0059874649759,3.02251039851757,2.17379573976275));
#9030=CARTESIAN_POINT('Ctrl Pts',(88.0035808828041,3.04897292264454,2.13652074716154));
#9031=CARTESIAN_POINT('Ctrl Pts',(87.9989644451124,3.09788237455742,2.06486734908438));
#9032=CARTESIAN_POINT('Ctrl Pts',(87.9967598932702,3.12046015448111,2.03058627490492));
#9033=CARTESIAN_POINT('Ctrl Pts',(87.990888679526,3.17852501389863,1.93916726351159));
#9034=CARTESIAN_POINT('Ctrl Pts',(87.9871882623625,3.21303729662564,1.88143070133032));
#9035=CARTESIAN_POINT('Ctrl Pts',(87.9692115249704,3.37079967232023,1.6004930987738));
#9036=CARTESIAN_POINT('Ctrl Pts',(87.9542264076569,3.47245280662494,1.36598264638312));
#9037=CARTESIAN_POINT('Ctrl Pts',(87.9282948771883,3.6049224318297,0.947287493582063));
#9038=CARTESIAN_POINT('Ctrl Pts',(87.9174353343064,3.64738881510277,0.767713351234325));
#9039=CARTESIAN_POINT('Ctrl Pts',(87.9048706635865,3.6826349352984,0.546485251920151));
#9040=CARTESIAN_POINT('Ctrl Pts',(87.9026678426373,3.68825791192327,0.507148916300196));
#9041=CARTESIAN_POINT('Ctrl Pts',(87.899090520988,3.69648295026552,0.442202865002715));
#9042=CARTESIAN_POINT('Ctrl Pts',(87.8976978945483,3.69945105548512,0.416643256640824));
#9043=CARTESIAN_POINT('Ctrl Pts',(87.8947839748211,3.70516712812947,0.362528428296357));
#9044=CARTESIAN_POINT('Ctrl Pts',(87.8932659257446,3.70785048885437,0.333968805923628));
#9045=CARTESIAN_POINT('Ctrl Pts',(87.888881714609,3.71471764158372,0.250536614950347));
#9046=CARTESIAN_POINT('Ctrl Pts',(87.8860583531453,3.71801534607256,0.195597076424892));
#9047=CARTESIAN_POINT('Ctrl Pts',(87.8717588336557,3.72870709199075,-0.0872884408589406));
#9048=CARTESIAN_POINT('Ctrl Pts',(87.860992463612,3.7163622370887,-0.315506229440126));
#9049=CARTESIAN_POINT('Ctrl Pts',(87.8412415427638,3.65656600417579,-0.722477350248943));
#9050=CARTESIAN_POINT('Ctrl Pts',(87.8323523753767,3.61657803567469,-0.90155673379347));
#9051=CARTESIAN_POINT('Ctrl Pts',(87.8196687619998,3.54407232004291,-1.14147362436956));
#9052=CARTESIAN_POINT('Ctrl Pts',(87.8162103016999,3.52282567848555,-1.20544978385056));
#9053=CARTESIAN_POINT('Ctrl Pts',(87.810319289663,3.48430696121762,-1.31169874820459));
#9054=CARTESIAN_POINT('Ctrl Pts',(87.8079169551383,3.46797247398676,-1.35429512504218));
#9055=CARTESIAN_POINT('Ctrl Pts',(87.8033002693359,3.43543249828027,-1.43469935700815));
#9056=CARTESIAN_POINT('Ctrl Pts',(87.8010910421485,3.41937503467993,-1.47255997705303));
#9057=CARTESIAN_POINT('Ctrl Pts',(87.7951866308746,3.37520571745417,-1.57208326169403));
#9058=CARTESIAN_POINT('Ctrl Pts',(87.7914569550663,3.34603267134391,-1.63325563680947));
#9059=CARTESIAN_POINT('Ctrl Pts',(87.773730122849,3.20155359473576,-1.91607299895188));
#9060=CARTESIAN_POINT('Ctrl Pts',(87.7590583907905,3.06580608880852,-2.1265193430973));
#9061=CARTESIAN_POINT('Ctrl Pts',(87.7331941842299,2.79265302044164,-2.46888231530573));
#9062=CARTESIAN_POINT('Ctrl Pts',(87.7220909587528,2.66427557913464,-2.60690167157309));
#9063=CARTESIAN_POINT('Ctrl Pts',(87.7093010454555,2.49677905294502,-2.76161991728417));
#9064=CARTESIAN_POINT('Ctrl Pts',(87.7070953033339,2.46712398390289,-2.78814449170409));
#9065=CARTESIAN_POINT('Ctrl Pts',(87.7035146682175,2.41759252376815,-2.83103803354901));
#9066=CARTESIAN_POINT('Ctrl Pts',(87.7021215794946,2.39796175684534,-2.84768493883956));
#9067=CARTESIAN_POINT('Ctrl Pts',(87.6992082732441,2.35610691025416,-2.88243808785088));
#9068=CARTESIAN_POINT('Ctrl Pts',(87.6976912673471,2.333843749245,-2.90049350268027));
#9069=CARTESIAN_POINT('Ctrl Pts',(87.6933137481492,2.26832297691828,-2.95238791855217));
#9070=CARTESIAN_POINT('Ctrl Pts',(87.6904958355666,2.22452103846253,-2.98553014947108));
#9071=CARTESIAN_POINT('Ctrl Pts',(87.6750641580192,1.97690499052962,-3.16440951635625));
#9072=CARTESIAN_POINT('Ctrl Pts',(87.6633127464237,1.75950191262105,-3.29026060598769));
#9073=CARTESIAN_POINT('Ctrl Pts',(87.6445062691672,1.40355007066605,-3.45086835914533));
#9074=CARTESIAN_POINT('Ctrl Pts',(87.6376923877593,1.27287491077724,-3.50117568379083));
#9075=CARTESIAN_POINT('Ctrl Pts',(87.6267604194912,1.06545880880276,-3.567876727291));
#9076=CARTESIAN_POINT('Ctrl Pts',(87.6227883416597,0.990504878425316,-3.58940745204731));
#9077=CARTESIAN_POINT('Ctrl Pts',(87.6162786327747,0.868875630176352,-3.62024589949874));
#9078=CARTESIAN_POINT('Ctrl Pts',(87.6137873848618,0.82260013944826,-3.63104034349186));
#9079=CARTESIAN_POINT('Ctrl Pts',(87.6089072603084,0.732573704330497,-3.65023107138224));
#9080=CARTESIAN_POINT('Ctrl Pts',(87.6065221549785,0.688853593681906,-3.65873360651626));
#9081=CARTESIAN_POINT('Ctrl Pts',(87.6006769001158,0.582445234716014,-3.67745270055126));
#9082=CARTESIAN_POINT('Ctrl Pts',(87.597192496409,0.519629271381674,-3.68685307164331));
#9083=CARTESIAN_POINT('Ctrl Pts',(87.5778301442832,0.174046608762157,-3.72956225635493));
#9084=CARTESIAN_POINT('Ctrl Pts',(87.5610214887244,-0.111552353881226,-3.73194837453821));
#9085=CARTESIAN_POINT('Ctrl Pts',(87.5352772026974,-0.545508079798557,-3.68569212844711));
#9086=CARTESIAN_POINT('Ctrl Pts',(87.5263747800677,-0.695321001251356,-3.66038799570502));
#9087=CARTESIAN_POINT('Ctrl Pts',(87.5152408535746,-0.887475551411152,-3.61570505316617));
#9088=CARTESIAN_POINT('Ctrl Pts',(87.5127056261594,-0.931582009343133,-3.60459307092547));
#9089=CARTESIAN_POINT('Ctrl Pts',(87.5087398558478,-1.00134789561889,-3.58565038412658));
#9090=CARTESIAN_POINT('Ctrl Pts',(87.5072832297286,-1.02714441683141,-3.57834608842259));
#9091=CARTESIAN_POINT('Ctrl Pts',(87.5043895968151,-1.07879365815488,-3.5631170057493));
#9092=CARTESIAN_POINT('Ctrl Pts',(87.5029529059371,-1.10464339838951,-3.55518798431808));
#9093=CARTESIAN_POINT('Ctrl Pts',(87.4990789703153,-1.17481109445507,-3.53282586792528));
#9094=CARTESIAN_POINT('Ctrl Pts',(87.496670438977,-1.21894920573821,-3.51784066240796));
#9095=CARTESIAN_POINT('Ctrl Pts',(87.4853492505099,-1.42798956971148,-3.44246284939659));
#9096=CARTESIAN_POINT('Ctrl Pts',(87.4768912872865,-1.5887753397043,-3.37127684563644));
#9097=CARTESIAN_POINT('Ctrl Pts',(87.4570953244919,-1.95347062775764,-3.17790241386006));
#9098=CARTESIAN_POINT('Ctrl Pts',(87.4458047703275,-2.15188629174054,-3.04704589493396));
#9099=CARTESIAN_POINT('Ctrl Pts',(87.4301565258806,-2.39389600829121,-2.85194042830058));
#9100=CARTESIAN_POINT('Ctrl Pts',(87.4263906576682,-2.44989885521468,-2.80397878159573));
#9101=CARTESIAN_POINT('Ctrl Pts',(87.4201306550807,-2.53902055178811,-2.72294450809819));
#9102=CARTESIAN_POINT('Ctrl Pts',(87.417676125414,-2.57300595649805,-2.69085344233467));
#9103=CARTESIAN_POINT('Ctrl Pts',(87.4128060618507,-2.63850301323551,-2.62663163530267));
#9104=CARTESIAN_POINT('Ctrl Pts',(87.4103929083172,-2.67005410918231,-2.59455250770431));
#9105=CARTESIAN_POINT('Ctrl Pts',(87.4043585211274,-2.74669040756521,-2.5137550646244));
#9106=CARTESIAN_POINT('Ctrl Pts',(87.4007091077082,-2.79106752677081,-2.46438917875553));
#9107=CARTESIAN_POINT('Ctrl Pts',(87.3823534203921,-3.00455537231326,-2.21373485841248));
#9108=CARTESIAN_POINT('Ctrl Pts',(87.3668830067885,-3.15331321311218,-1.99613532522483));
#9109=CARTESIAN_POINT('Ctrl Pts',(87.3416509594145,-3.3559048006028,-1.61983012253875));
#9110=CARTESIAN_POINT('Ctrl Pts',(87.3319647392225,-3.42422324419902,-1.46991448869948));
#9111=CARTESIAN_POINT('Ctrl Pts',(87.3200127521161,-3.4989813131001,-1.27208394646723));
#9112=CARTESIAN_POINT('Ctrl Pts',(87.3173947588679,-3.51473241462857,-1.2278942309448));
#9113=CARTESIAN_POINT('Ctrl Pts',(87.3133314728247,-3.53825873204522,-1.1577249143893));
#9114=CARTESIAN_POINT('Ctrl Pts',(87.311858021571,-3.54659216653548,-1.13193901168864));
#9115=CARTESIAN_POINT('Ctrl Pts',(87.3089620675417,-3.56259210515531,-1.08051875309074));
#9116=CARTESIAN_POINT('Ctrl Pts',(87.3075393156371,-3.57026526575852,-1.05488828208453));
#9117=CARTESIAN_POINT('Ctrl Pts',(87.3037510938621,-3.59015699470958,-0.985739925626268));
#9118=CARTESIAN_POINT('Ctrl Pts',(87.3014121936805,-3.60186077134007,-0.942077371476803));
#9119=CARTESIAN_POINT('Ctrl Pts',(87.2863192786097,-3.67322439539774,-0.65503989190597));
#9120=CARTESIAN_POINT('Ctrl Pts',(87.2745319491281,-3.70898210585364,-0.406363048817564));
#9121=CARTESIAN_POINT('Ctrl Pts',(87.2562721399099,-3.72490374872104,-0.0266501069281622));
#9122=CARTESIAN_POINT('Ctrl Pts',(87.2500057611676,-3.72357860408172,0.102850190824901));
#9123=CARTESIAN_POINT('Ctrl Pts',(87.238928349933,-3.70967572988444,0.325493722224022));
#9124=CARTESIAN_POINT('Ctrl Pts',(87.2341985579693,-3.70031298148294,0.418715085825928));
#9125=CARTESIAN_POINT('Ctrl Pts',(87.2267679865319,-3.68053254130884,0.561319448893375));
#9126=CARTESIAN_POINT('Ctrl Pts',(87.2241421221132,-3.67260990985818,0.611011822737596));
#9127=CARTESIAN_POINT('Ctrl Pts',(87.2191521944317,-3.65584337743535,0.704009182172894));
#9128=CARTESIAN_POINT('Ctrl Pts',(87.2167956392945,-3.64723069725869,0.747347139286704));
#9129=CARTESIAN_POINT('Ctrl Pts',(87.2113778000089,-3.62587872103958,0.845605538925054));
#9130=CARTESIAN_POINT('Ctrl Pts',(87.2083021192094,-3.61265932591186,0.900409548344087));
#9131=CARTESIAN_POINT('Ctrl Pts',(87.1978515838246,-3.56412586457384,1.08329248893044));
#9132=CARTESIAN_POINT('Ctrl Pts',(87.1903089898278,-3.52320500320499,1.20976725898419));
#9133=CARTESIAN_POINT('Ctrl Pts',(87.1689867403307,-3.39126144318707,1.55359210349915));
#9134=CARTESIAN_POINT('Ctrl Pts',(87.154906767161,-3.28624325195498,1.76490753501621));
#9135=CARTESIAN_POINT('Ctrl Pts',(87.1369820493023,-3.12408132064938,2.02586788704766));
#9136=CARTESIAN_POINT('Ctrl Pts',(87.1328317942871,-3.08441911274939,2.0857575187262));
#9137=CARTESIAN_POINT('Ctrl Pts',(87.1257644639136,-3.01274413640612,2.18746605764376));
#9138=CARTESIAN_POINT('Ctrl Pts',(87.1228153393004,-2.98153105680148,2.22982243141839));
#9139=CARTESIAN_POINT('Ctrl Pts',(87.1183644403625,-2.93220890175546,2.29386464656165));
#9140=CARTESIAN_POINT('Ctrl Pts',(87.1168256235655,-2.91473429248608,2.31602853269854));
#9141=CARTESIAN_POINT('Ctrl Pts',(87.1139217341,-2.88090433879447,2.35794726614331));
#9142=CARTESIAN_POINT('Ctrl Pts',(87.1125540829754,-2.86459413087463,2.37773539443057));
#9143=CARTESIAN_POINT('Ctrl Pts',(87.1090495928073,-2.82186335034614,2.42849999482197));
#9144=CARTESIAN_POINT('Ctrl Pts',(87.106933070194,-2.79513598764554,2.45921533469826));
#9145=CARTESIAN_POINT('Ctrl Pts',(87.1012014979304,-2.72043575025773,2.54226997610862));
#9146=CARTESIAN_POINT('Ctrl Pts',(87.0976455027076,-2.67148468059826,2.59365907861286));
#9147=CARTESIAN_POINT('Ctrl Pts',(87.0941439893651,-2.62112000711957,2.64359555733806));
#9148=CARTESIAN_POINT('Ctrl Pts',(86.8469367975355,-2.62112000731897,2.64359555714035));
#9149=CARTESIAN_POINT('Ctrl Pts',(86.8473899349745,-2.62706139976061,2.63770467774389));
#9150=CARTESIAN_POINT('Ctrl Pts',(86.8478439237163,-2.63298296180103,2.63179374004676));
#9151=CARTESIAN_POINT('Ctrl Pts',(86.8522648269433,-2.69034510248191,2.57414713842212));
#9152=CARTESIAN_POINT('Ctrl Pts',(86.8562945859776,-2.74027159920205,2.52093253104793));
#9153=CARTESIAN_POINT('Ctrl Pts',(86.8654083654593,-2.84797960956079,2.39914845539768));
#9154=CARTESIAN_POINT('Ctrl Pts',(86.8705201335773,-2.90491158070205,2.32989018388121));
#9155=CARTESIAN_POINT('Ctrl Pts',(86.8894238697966,-3.10337451565115,2.06986359556756));
#9156=CARTESIAN_POINT('Ctrl Pts',(86.9036213542172,-3.22906402916566,1.86772681932388));
#9157=CARTESIAN_POINT('Ctrl Pts',(86.9237344933729,-3.38214556663351,1.55928838810713));
#9158=CARTESIAN_POINT('Ctrl Pts',(86.9298940203282,-3.42551618219064,1.46155088764665));
#9159=CARTESIAN_POINT('Ctrl Pts',(86.937903803101,-3.47797564028516,1.32811324295582));
#9160=CARTESIAN_POINT('Ctrl Pts',(86.939919987003,-3.49082824486581,1.29395428999919));
#9161=CARTESIAN_POINT('Ctrl Pts',(86.9432804599939,-3.51169022498739,1.23593381450495));
#9162=CARTESIAN_POINT('Ctrl Pts',(86.94463865535,-3.51996345481526,1.21217079316765));
#9163=CARTESIAN_POINT('Ctrl Pts',(86.9475820335882,-3.53755079811137,1.15995601156604));
#9164=CARTESIAN_POINT('Ctrl Pts',(86.9491618493022,-3.54676366908233,1.13147301686612));
#9165=CARTESIAN_POINT('Ctrl Pts',(86.9539823311102,-3.57411596005467,1.04329062954808));
#9166=CARTESIAN_POINT('Ctrl Pts',(86.9571659275947,-3.59109964713755,0.983241762208478));
#9167=CARTESIAN_POINT('Ctrl Pts',(86.9649254941717,-3.62942355092949,0.833459573771509));
#9168=CARTESIAN_POINT('Ctrl Pts',(86.9694375816899,-3.64895452789624,0.743305155814841));
#9169=CARTESIAN_POINT('Ctrl Pts',(86.984682524476,-3.70416359584887,0.433200717531767));
#9170=CARTESIAN_POINT('Ctrl Pts',(86.9951748666698,-3.72344507782224,0.210828040851256));
#9171=CARTESIAN_POINT('Ctrl Pts',(87.0118083870354,-3.72235777203515,-0.128304325582148));
#9172=CARTESIAN_POINT('Ctrl Pts',(87.017618646654,-3.71652864138321,-0.244583929871908));
#9173=CARTESIAN_POINT('Ctrl Pts',(87.0263791707301,-3.6999958379374,-0.414560098068529));
#9174=CARTESIAN_POINT('Ctrl Pts',(87.0292039653643,-3.69354043233271,-0.468602134953449));
#9175=CARTESIAN_POINT('Ctrl Pts',(87.0343673135872,-3.67975601811787,-0.565845783029031));
#9176=CARTESIAN_POINT('Ctrl Pts',(87.0366927238313,-3.67284448532002,-0.60909685082763));
#9177=CARTESIAN_POINT('Ctrl Pts',(87.0418271086227,-3.6560733939613,-0.703343308434649));
#9178=CARTESIAN_POINT('Ctrl Pts',(87.044645117817,-3.64590658019617,-0.75427403098112));
#9179=CARTESIAN_POINT('Ctrl Pts',(87.0532226561584,-3.61211666853835,-0.906844780102981));
#9180=CARTESIAN_POINT('Ctrl Pts',(87.0590780729086,-3.58528411650565,-1.00771488732806));
#9181=CARTESIAN_POINT('Ctrl Pts',(87.0738703301397,-3.50830042704802,-1.25481575578491));
#9182=CARTESIAN_POINT('Ctrl Pts',(87.0829257819692,-3.45321429435865,-1.39929973263157));
#9183=CARTESIAN_POINT('Ctrl Pts',(87.1044709741835,-3.30217946521773,-1.73171955214702));
#9184=CARTESIAN_POINT('Ctrl Pts',(87.1169832392531,-3.19891671648481,-1.91577225783769));
#9185=CARTESIAN_POINT('Ctrl Pts',(87.131342122091,-3.055880654736,-2.12659468478338));
#9186=CARTESIAN_POINT('Ctrl Pts',(87.13379710035,-3.03047911295223,-2.16263917643575));
#9187=CARTESIAN_POINT('Ctrl Pts',(87.1376642862929,-2.98882080052086,-2.21957600955985));
#9188=CARTESIAN_POINT('Ctrl Pts',(87.139100675472,-2.97297167492617,-2.24076035516961));
#9189=CARTESIAN_POINT('Ctrl Pts',(87.141979966135,-2.94039885077346,-2.28334394995256));
#9190=CARTESIAN_POINT('Ctrl Pts',(87.1434220714834,-2.92366425503528,-2.30473261094895));
#9191=CARTESIAN_POINT('Ctrl Pts',(87.147350631069,-2.87697309610368,-2.36308201632092));
#9192=CARTESIAN_POINT('Ctrl Pts',(87.1498067998886,-2.84653897727171,-2.39965561167959));
#9193=CARTESIAN_POINT('Ctrl Pts',(87.1554057637012,-2.7745569909931,-2.48286129514672));
#9194=CARTESIAN_POINT('Ctrl Pts',(87.1585224419049,-2.73251970072881,-2.52905188247201));
#9195=CARTESIAN_POINT('Ctrl Pts',(87.1700258842128,-2.57109607692522,-2.69769795905632));
#9196=CARTESIAN_POINT('Ctrl Pts',(87.1781497407726,-2.44447781565016,-2.81294190932959));
#9197=CARTESIAN_POINT('Ctrl Pts',(87.1953722239273,-2.16303389795497,-3.03569824269789));
#9198=CARTESIAN_POINT('Ctrl Pts',(87.2044691642374,-2.00707626905943,-3.1409897970051));
#9199=CARTESIAN_POINT('Ctrl Pts',(87.2174288270614,-1.78438228839504,-3.26795545598925));
#9200=CARTESIAN_POINT('Ctrl Pts',(87.2209380423758,-1.72399646643795,-3.30021036674723));
#9201=CARTESIAN_POINT('Ctrl Pts',(87.2268815658895,-1.6219157348871,-3.35117005119017));
#9202=CARTESIAN_POINT('Ctrl Pts',(87.2292839992155,-1.58070312253751,-3.37080535797707));
#9203=CARTESIAN_POINT('Ctrl Pts',(87.2341641362162,-1.49716651676246,-3.40873658367422));
#9204=CARTESIAN_POINT('Ctrl Pts',(87.2366419191941,-1.45484296903431,-3.42701391238433));
#9205=CARTESIAN_POINT('Ctrl Pts',(87.2430014108148,-1.34650799464527,-3.47142958889346));
#9206=CARTESIAN_POINT('Ctrl Pts',(87.2469175851446,-1.28007027387451,-3.49647341522531));
#9207=CARTESIAN_POINT('Ctrl Pts',(87.2557181200866,-1.1314156173652,-3.5477042615272));
#9208=CARTESIAN_POINT('Ctrl Pts',(87.2606271783031,-1.04892349588877,-3.57296303828486));
#9209=CARTESIAN_POINT('Ctrl Pts',(87.2780359194904,-0.7573864219849,-3.65126389773269));
#9210=CARTESIAN_POINT('Ctrl Pts',(87.2908705554386,-0.544682061964044,-3.68899360794475));
#9211=CARTESIAN_POINT('Ctrl Pts',(87.3113060964913,-0.198259845136661,-3.71981640525909));
#9212=CARTESIAN_POINT('Ctrl Pts',(87.3189883217274,-0.0660517408872298,
-3.7245111635414));
#9213=CARTESIAN_POINT('Ctrl Pts',(87.3285327134508,0.104382164702472,-3.72148294148486));
#9214=CARTESIAN_POINT('Ctrl Pts',(87.3306504181745,0.142618747206788,-3.72021384322786));
#9215=CARTESIAN_POINT('Ctrl Pts',(87.3341118551425,0.205956205848665,-3.71713362724989));
#9216=CARTESIAN_POINT('Ctrl Pts',(87.335472092754,0.231069883848536,-3.7156570350764));
#9217=CARTESIAN_POINT('Ctrl Pts',(87.3383670199711,0.285041684580131,-3.71193432525252));
#9218=CARTESIAN_POINT('Ctrl Pts',(87.3398975313162,0.313891695691506,-3.70960608486964));
#9219=CARTESIAN_POINT('Ctrl Pts',(87.3443859500546,0.399303504323378,-3.70170963038285));
#9220=CARTESIAN_POINT('Ctrl Pts',(87.3472976685906,0.455770077201023,-3.69518223395162));
#9221=CARTESIAN_POINT('Ctrl Pts',(87.3542148388467,0.591635461779865,-3.67631448184335));
#9222=CARTESIAN_POINT('Ctrl Pts',(87.3581732040126,0.670828372940872,-3.66269178521249));
#9223=CARTESIAN_POINT('Ctrl Pts',(87.3695118136425,0.898987413466158,-3.61579494022049));
#9224=CARTESIAN_POINT('Ctrl Pts',(87.3767616091401,1.04642569633715,-3.57591200447481));
#9225=CARTESIAN_POINT('Ctrl Pts',(87.3924580917532,1.35586109260056,-3.47142413618571));
#9226=CARTESIAN_POINT('Ctrl Pts',(87.4009153350006,1.51660414695282,-3.40426940925044));
#9227=CARTESIAN_POINT('Ctrl Pts',(87.413151299323,1.73275126561451,-3.29561162782169));
#9228=CARTESIAN_POINT('Ctrl Pts',(87.4166354898917,1.79260063763816,-3.26344376179476));
#9229=CARTESIAN_POINT('Ctrl Pts',(87.4223123148643,1.88711627543246,-3.20925878064477));
#9230=CARTESIAN_POINT('Ctrl Pts',(87.42446920123,1.92235780184505,-3.18827383797709));
#9231=CARTESIAN_POINT('Ctrl Pts',(87.4290528771893,1.99579526723477,-3.14288445497222));
#9232=CARTESIAN_POINT('Ctrl Pts',(87.4314838425139,2.03390646803325,-3.11835624694404));
#9233=CARTESIAN_POINT('Ctrl Pts',(87.4375462680497,2.12684690719819,-3.05611150919702));
#9234=CARTESIAN_POINT('Ctrl Pts',(87.4412058104457,2.18112920342523,-3.017609974659));
#9235=CARTESIAN_POINT('Ctrl Pts',(87.4548399513917,2.37669539652386,-2.87086365347971));
#9236=CARTESIAN_POINT('Ctrl Pts',(87.4651234889337,2.511185373091,-2.7539926250342));
#9237=CARTESIAN_POINT('Ctrl Pts',(87.4904133442831,2.81511217352789,-2.44904506187802));
#9238=CARTESIAN_POINT('Ctrl Pts',(87.5055487981762,2.97476267811515,-2.25243709313934));
#9239=CARTESIAN_POINT('Ctrl Pts',(87.5223244904424,3.13784274550207,-2.00370111649192));
#9240=CARTESIAN_POINT('Ctrl Pts',(87.5248209754313,3.16173304057958,-1.9657873198146));
#9241=CARTESIAN_POINT('Ctrl Pts',(87.5287370172134,3.19870503329672,-1.90469449549014));
#9242=CARTESIAN_POINT('Ctrl Pts',(87.5301817666119,3.21223229639277,-1.88179137674653));
#9243=CARTESIAN_POINT('Ctrl Pts',(87.5330610185432,3.23899009311629,-1.83535808010318));
#9244=CARTESIAN_POINT('Ctrl Pts',(87.534495039195,3.25221245292654,-1.81182514440652));
#9245=CARTESIAN_POINT('Ctrl Pts',(87.5383739224393,3.28763712018424,-1.74713937349005));
#9246=CARTESIAN_POINT('Ctrl Pts',(87.540789769645,3.30932250483166,-1.70570770003931));
#9247=CARTESIAN_POINT('Ctrl Pts',(87.5515227723301,3.40350230651728,-1.51720834710164));
#9248=CARTESIAN_POINT('Ctrl Pts',(87.5594486119933,3.46701881599291,-1.36584699771955));
#9249=CARTESIAN_POINT('Ctrl Pts',(87.5799943253291,3.60621670591948,-0.961128375247433));
#9250=CARTESIAN_POINT('Ctrl Pts',(87.5925193231542,3.66527614170109,-0.703070443728016));
#9251=CARTESIAN_POINT('Ctrl Pts',(87.6092424466115,3.70437464903941,-0.375295410529423));
#9252=CARTESIAN_POINT('Ctrl Pts',(87.6126376483127,3.71045476337085,-0.309455923773697));
#9253=CARTESIAN_POINT('Ctrl Pts',(87.6184219342769,3.71770851794193,-0.198790640705265));
#9254=CARTESIAN_POINT('Ctrl Pts',(87.6207819924242,3.71983135528355,-0.154041565688244));
#9255=CARTESIAN_POINT('Ctrl Pts',(87.6256423167465,3.72251100625336,-0.0627840324924113));
#9256=CARTESIAN_POINT('Ctrl Pts',(87.6281440655121,3.72300479016126,-0.0162817801131505));
#9257=CARTESIAN_POINT('Ctrl Pts',(87.6346530902917,3.72203305449251,0.103435917079885));
#9258=CARTESIAN_POINT('Ctrl Pts',(87.6386981812944,3.7192786903159,0.176618412499463));
#9259=CARTESIAN_POINT('Ctrl Pts',(87.6478545169702,3.70832644558581,0.339556927789161));
#9260=CARTESIAN_POINT('Ctrl Pts',(87.6529939378152,3.6990238332021,0.429191084747156));
#9261=CARTESIAN_POINT('Ctrl Pts',(87.6721183090258,3.65295445052668,0.756805650929006));
#9262=CARTESIAN_POINT('Ctrl Pts',(87.6865199576498,3.59638014142236,0.991398050306722));
#9263=CARTESIAN_POINT('Ctrl Pts',(87.7065985183614,3.48371450341881,1.31654396977808));
#9264=CARTESIAN_POINT('Ctrl Pts',(87.7125491408456,3.44581064111291,1.41277979517627));
#9265=CARTESIAN_POINT('Ctrl Pts',(87.7203414801692,3.38930755174152,1.54037956989887));
#9266=CARTESIAN_POINT('Ctrl Pts',(87.7223382706663,3.37418632449789,1.57322653852528));
#9267=CARTESIAN_POINT('Ctrl Pts',(87.7256771808073,3.34775228223228,1.62851259482424));
#9268=CARTESIAN_POINT('Ctrl Pts',(87.7270327616913,3.33668686240006,1.65106617637407));
#9269=CARTESIAN_POINT('Ctrl Pts',(87.7299833884142,3.31185024873655,1.70041850411334));
#9270=CARTESIAN_POINT('Ctrl Pts',(87.7315727822955,3.29798079244825,1.72716471941759));
#9271=CARTESIAN_POINT('Ctrl Pts',(87.7364598834056,3.2538675110606,1.8097645428743));
#9272=CARTESIAN_POINT('Ctrl Pts',(87.7396982039293,3.22251685282666,1.86501674445612));
#9273=CARTESIAN_POINT('Ctrl Pts',(87.7476331619983,3.14092599293388,2.00060599787278));
#9274=CARTESIAN_POINT('Ctrl Pts',(87.7522620855194,3.08900346766987,2.07987971926953));
#9275=CARTESIAN_POINT('Ctrl Pts',(87.7718710877152,2.85400839829867,2.41041824362851));
#9276=CARTESIAN_POINT('Ctrl Pts',(87.786415500584,2.64290191557751,2.64017927228636));
#9277=CARTESIAN_POINT('Ctrl Pts',(87.8054413772444,2.35686525737934,2.88238583047108));
#9278=CARTESIAN_POINT('Ctrl Pts',(87.8087330175567,2.30697716961592,2.92246773244327));
#9279=CARTESIAN_POINT('Ctrl Pts',(87.8143953933482,2.22072124691013,2.98818355318106));
#9280=CARTESIAN_POINT('Ctrl Pts',(87.8167400435671,2.18488112487688,3.01448802472819));
#9281=CARTESIAN_POINT('Ctrl Pts',(87.8216166108929,2.11015236783528,3.06730154094434));
#9282=CARTESIAN_POINT('Ctrl Pts',(87.8241510134052,2.07121501682897,3.09372749939246));
#9283=CARTESIAN_POINT('Ctrl Pts',(87.8308629366755,1.96789795484324,3.16102181846558));
#9284=CARTESIAN_POINT('Ctrl Pts',(87.8350829761815,1.90274755190945,3.20066116879983));
#9285=CARTESIAN_POINT('Ctrl Pts',(87.8477814453308,1.70618579254025,3.31213169953281));
#9286=CARTESIAN_POINT('Ctrl Pts',(87.8564383143798,1.57161604328785,3.37806195957758));
#9287=CARTESIAN_POINT('Ctrl Pts',(87.8807836924883,1.18859066375219,3.53786860470293));
#9288=CARTESIAN_POINT('Ctrl Pts',(87.8967136362589,0.933506570284459,3.61356258857102));
#9289=CARTESIAN_POINT('Ctrl Pts',(87.9140467192536,0.630578803360852,3.66920400504446));
#9290=CARTESIAN_POINT('Ctrl Pts',(87.9164190809944,0.588487007166788,3.67618973996398));
#9291=CARTESIAN_POINT('Ctrl Pts',(87.9201892596059,0.520389131938299,3.68629189672736));
#9292=CARTESIAN_POINT('Ctrl Pts',(87.9216092707534,0.494454620036324,3.68986009884771));
#9293=CARTESIAN_POINT('Ctrl Pts',(87.9244907451265,0.4411837282703,3.69661760871857));
#9294=CARTESIAN_POINT('Ctrl Pts',(87.9259507429193,0.413845666194757,3.6997779235437));
#9295=CARTESIAN_POINT('Ctrl Pts',(87.929989923136,0.337347535583371,3.7077626584229));
#9296=CARTESIAN_POINT('Ctrl Pts',(87.9325359113087,0.288121415849994,3.71191241466898));
#9297=CARTESIAN_POINT('Ctrl Pts',(87.9383865952892,0.173168811171942,3.71930217894022));
#9298=CARTESIAN_POINT('Ctrl Pts',(87.94166166476,0.107409295024827,3.72178184391183));
#9299=CARTESIAN_POINT('Ctrl Pts',(87.9542963132215,-0.149666044005904,3.72465583143753));
#9300=CARTESIAN_POINT('Ctrl Pts',(87.9633404188895,-0.340834509650255,3.71204770811981));
#9301=CARTESIAN_POINT('Ctrl Pts',(87.9811734316564,-0.707499832718931,3.65928959122063));
#9302=CARTESIAN_POINT('Ctrl Pts',(87.9899197054762,-0.882722593028811,3.6210149663471));
#9303=CARTESIAN_POINT('Ctrl Pts',(88.0021233170764,-1.11247135391488,3.55315762055016));
#9304=CARTESIAN_POINT('Ctrl Pts',(88.0052422536444,-1.1700162574781,3.53462629232209));
#9305=CARTESIAN_POINT('Ctrl Pts',(88.0107276247342,-1.26897764421147,3.50007606229411));
#9306=CARTESIAN_POINT('Ctrl Pts',(88.0130731675355,-1.31060659683479,3.48470182783606));
#9307=CARTESIAN_POINT('Ctrl Pts',(88.0180275870966,-1.39704225674514,3.45101184348976));
#9308=CARTESIAN_POINT('Ctrl Pts',(88.0206405852091,-1.44178630984336,3.43255906743687));
#9309=CARTESIAN_POINT('Ctrl Pts',(88.027844680944,-1.56280222561935,3.3798676052861));
#9310=CARTESIAN_POINT('Ctrl Pts',(88.032490539931,-1.638297560711,3.34392515592509));
#9311=CARTESIAN_POINT('Ctrl Pts',(88.0521474877394,-1.94731673693956,3.18382705588358));
#9312=CARTESIAN_POINT('Ctrl Pts',(88.0678516829027,-2.16846840066719,3.03751754194363));
#9313=CARTESIAN_POINT('Ctrl Pts',(88.0900120865799,-2.45854736152291,2.79767011230306));
#9314=CARTESIAN_POINT('Ctrl Pts',(88.0965584132985,-2.541596160395,2.72244330185412));
#9315=CARTESIAN_POINT('Ctrl Pts',(88.1029424533549,-2.62112001609809,2.64359554843587));
#9316=CARTESIAN_POINT('Origin',(80.1322559480305,0.,0.));
#9317=CARTESIAN_POINT('',(89.5984125828093,-2.62112000687686,2.6435955575787));
#9318=CARTESIAN_POINT('',(89.3487674494621,-2.62112000711956,2.64359555733806));
#9319=CARTESIAN_POINT('',(80.1322559480305,-2.62112000711956,2.64359555733806));
#9320=CARTESIAN_POINT('Ctrl Pts',(89.5984125828093,-2.62112000663417,2.64359555781933));
#9321=CARTESIAN_POINT('Ctrl Pts',(89.5943271447616,-2.5618080717952,2.70240322927981));
#9322=CARTESIAN_POINT('Ctrl Pts',(89.5901926787951,-2.50053473596257,2.75919725800358));
#9323=CARTESIAN_POINT('Ctrl Pts',(89.5822945568946,-2.38202439419345,2.86185173325579));
#9324=CARTESIAN_POINT('Ctrl Pts',(89.5785496786393,-2.32524350402295,2.90817422540554));
#9325=CARTESIAN_POINT('Ctrl Pts',(89.5723142085096,-2.23011948428828,2.98120990868023));
#9326=CARTESIAN_POINT('Ctrl Pts',(89.5698624397723,-2.1925739153427,3.0089308407746));
#9327=CARTESIAN_POINT('Ctrl Pts',(89.5649901827266,-2.11776324134503,3.06202183484714));
#9328=CARTESIAN_POINT('Ctrl Pts',(89.562571907531,-2.08053876462607,3.0874353553927));
#9329=CARTESIAN_POINT('Ctrl Pts',(89.5565104335751,-1.98706422803676,3.14879316191372));
#9330=CARTESIAN_POINT('Ctrl Pts',(89.5528385141918,-1.93029301021984,3.18391123407403));
#9331=CARTESIAN_POINT('Ctrl Pts',(89.5343776809933,-1.64427933930165,3.35037437243731));
#9332=CARTESIAN_POINT('Ctrl Pts',(89.5188149771131,-1.40247738177234,3.45856688682408));
#9333=CARTESIAN_POINT('Ctrl Pts',(89.4933721941459,-0.993160166882023,3.59167855485942));
#9334=CARTESIAN_POINT('Ctrl Pts',(89.4835709032494,-0.83173765598187,3.6324566666028));
#9335=CARTESIAN_POINT('Ctrl Pts',(89.4715019718314,-0.621798218042232,3.6707562904483));
#9336=CARTESIAN_POINT('Ctrl Pts',(89.4688723455797,-0.575317235283083,3.67832777848009));
#9337=CARTESIAN_POINT('Ctrl Pts',(89.464798557957,-0.501903698917201,3.68886069567858));
#9338=CARTESIAN_POINT('Ctrl Pts',(89.4633257551182,-0.475062309323462,3.69241336352804));
#9339=CARTESIAN_POINT('Ctrl Pts',(89.4604433012178,-0.421872711140325,3.69886380255716));
#9340=CARTESIAN_POINT('Ctrl Pts',(89.4590331920707,-0.395527805133241,3.70177360594109));
#9341=CARTESIAN_POINT('Ctrl Pts',(89.4552986738902,-0.324976102185999,3.70880427079457));
#9342=CARTESIAN_POINT('Ctrl Pts',(89.4529998739697,-0.280721626942598,3.71241623237597));
#9343=CARTESIAN_POINT('Ctrl Pts',(89.4377034636118,0.0182346209747569,3.73143969417713));
#9344=CARTESIAN_POINT('Ctrl Pts',(89.4257234248191,0.273896898122981,3.72142194754956));
#9345=CARTESIAN_POINT('Ctrl Pts',(89.4049751944012,0.701512062560916,3.66032612678257));
#9346=CARTESIAN_POINT('Ctrl Pts',(89.3963859606162,0.874467693343638,3.62290020498499));
#9347=CARTESIAN_POINT('Ctrl Pts',(89.3840783653783,1.10779716648023,3.55472314485318));
#9348=CARTESIAN_POINT('Ctrl Pts',(89.380672045639,1.17098193445921,3.53441251582577));
#9349=CARTESIAN_POINT('Ctrl Pts',(89.3748522765092,1.27629864743267,3.49742455879786));
#9350=CARTESIAN_POINT('Ctrl Pts',(89.3724678820671,1.31873094876546,3.48164691358501));
#9351=CARTESIAN_POINT('Ctrl Pts',(89.3678751547635,1.39903377573888,3.45010923326288));
#9352=CARTESIAN_POINT('Ctrl Pts',(89.3656716891562,1.43695233626936,3.43448934043742));
#9353=CARTESIAN_POINT('Ctrl Pts',(89.3597588301606,1.53705241603428,3.39130697012417));
#9354=CARTESIAN_POINT('Ctrl Pts',(89.3560142559021,1.59874770073665,3.36266234819664));
#9355=CARTESIAN_POINT('Ctrl Pts',(89.3424350497237,1.81641827523252,3.25425499992135));
#9356=CARTESIAN_POINT('Ctrl Pts',(89.3323054185756,1.96749236243847,3.1652035561517));
#9357=CARTESIAN_POINT('Ctrl Pts',(89.3113307670147,2.26141386177886,2.96275420499678));
#9358=CARTESIAN_POINT('Ctrl Pts',(89.300501553853,2.40335113914105,2.84882590155623));
#9359=CARTESIAN_POINT('Ctrl Pts',(89.2861985663028,2.5834569035375,2.68118461925042));
#9360=CARTESIAN_POINT('Ctrl Pts',(89.2824983910797,2.62937429390787,2.63616996086165));
#9361=CARTESIAN_POINT('Ctrl Pts',(89.2761074655527,2.70790401280267,2.55508974984062));
#9362=CARTESIAN_POINT('Ctrl Pts',(89.2733916289446,2.74101865568885,2.51953268185867));
#9363=CARTESIAN_POINT('Ctrl Pts',(89.2692181405706,2.7916720871035,2.46296212279386));
#9364=CARTESIAN_POINT('Ctrl Pts',(89.267729578352,2.80969045020819,2.44238717781868));
#9365=CARTESIAN_POINT('Ctrl Pts',(89.2648342479026,2.84468102692327,2.40153213123823));
#9366=CARTESIAN_POINT('Ctrl Pts',(89.2634266093837,2.86166698599168,2.38126622728695));
#9367=CARTESIAN_POINT('Ctrl Pts',(89.259737617861,2.90605210688444,2.3271495667082));
#9368=CARTESIAN_POINT('Ctrl Pts',(89.2574803451724,2.9330764566551,2.29299515105011));
#9369=CARTESIAN_POINT('Ctrl Pts',(89.2419237087941,3.11764829601166,2.05112205328567));
#9370=CARTESIAN_POINT('Ctrl Pts',(89.2296902411884,3.25360833024745,1.82781101317892));
#9371=CARTESIAN_POINT('Ctrl Pts',(89.2099146921086,3.42945410741587,1.4561379406622));
#9372=CARTESIAN_POINT('Ctrl Pts',(89.2026052257,3.48548030831931,1.31640269209036));
#9373=CARTESIAN_POINT('Ctrl Pts',(89.1911544044757,3.5574065486287,1.0998951742217));
#9374=CARTESIAN_POINT('Ctrl Pts',(89.187193005777,3.57959695857387,1.02537570048041));
#9375=CARTESIAN_POINT('Ctrl Pts',(89.1806917497927,3.61157702884788,0.904234949720744));
#9376=CARTESIAN_POINT('Ctrl Pts',(89.1781977102319,3.6228337593404,0.858023754605999));
#9377=CARTESIAN_POINT('Ctrl Pts',(89.1733053945656,3.64294860031054,0.767979035047733));
#9378=CARTESIAN_POINT('Ctrl Pts',(89.1709107515881,3.65190833694855,0.724176476745814));
#9379=CARTESIAN_POINT('Ctrl Pts',(89.1650281296726,3.67177254526394,0.617293325350234));
#9380=CARTESIAN_POINT('Ctrl Pts',(89.1615153958727,3.68184275931097,0.554073904307277));
#9381=CARTESIAN_POINT('Ctrl Pts',(89.1398253282955,3.73323708455912,0.167510083016139));
#9382=CARTESIAN_POINT('Ctrl Pts',(89.1203886395769,3.73356572176802,-0.159819337753641));
#9383=CARTESIAN_POINT('Ctrl Pts',(89.0962884968879,3.680240688744,-0.567410937842279));
#9384=CARTESIAN_POINT('Ctrl Pts',(89.0913339933252,3.66629067271162,-0.651491111261201));
#9385=CARTESIAN_POINT('Ctrl Pts',(89.0830910000021,3.63777258928263,-0.793086656427543));
#9386=CARTESIAN_POINT('Ctrl Pts',(89.0797563563629,3.62469329085107,-0.850867281344274));
#9387=CARTESIAN_POINT('Ctrl Pts',(89.0748566634192,3.60303802061444,-0.936939635855264));
#9388=CARTESIAN_POINT('Ctrl Pts',(89.07324333015,3.5954955463849,-0.965479542648749));
#9389=CARTESIAN_POINT('Ctrl Pts',(89.0702707695591,3.58080465612314,-1.01850679064977));
#9390=CARTESIAN_POINT('Ctrl Pts',(89.0689074038154,3.57374283771589,-1.04301496428459));
#9391=CARTESIAN_POINT('Ctrl Pts',(89.0655409037207,3.55550500125024,-1.10394896451903));
#9392=CARTESIAN_POINT('Ctrl Pts',(89.0635541446008,3.54402040381528,-1.14028010784235));
#9393=CARTESIAN_POINT('Ctrl Pts',(89.0550405017232,3.49177317004527,-1.29714127939003));
#9394=CARTESIAN_POINT('Ctrl Pts',(89.0487689976239,3.44540155202557,-1.41572189261893));
#9395=CARTESIAN_POINT('Ctrl Pts',(89.031957226059,3.30277196959761,-1.73167653153313));
#9396=CARTESIAN_POINT('Ctrl Pts',(89.0216261014067,3.19499827980722,-1.92327693488621));
#9397=CARTESIAN_POINT('Ctrl Pts',(89.0066481876398,3.02183548524199,-2.17599087775461));
#9398=CARTESIAN_POINT('Ctrl Pts',(89.0023440689527,2.9701981383992,-2.24596257615318));
#9399=CARTESIAN_POINT('Ctrl Pts',(88.9943565522433,2.87174779334856,-2.37002894411395));
#9400=CARTESIAN_POINT('Ctrl Pts',(88.9907010319644,2.82573477310012,-2.42470508581248));
#9401=CARTESIAN_POINT('Ctrl Pts',(88.9845744622068,2.74734510282089,-2.51258992862816));
#9402=CARTESIAN_POINT('Ctrl Pts',(88.9821395595911,2.71586984457589,-2.54657888168349));
#9403=CARTESIAN_POINT('Ctrl Pts',(88.977242835758,2.65200519511514,-2.61301296685249));
#9404=CARTESIAN_POINT('Ctrl Pts',(88.9747819940956,2.61963443281089,-2.64546470534321));
#9405=CARTESIAN_POINT('Ctrl Pts',(88.968568792321,2.53727299727478,-2.72503793078099));
#9406=CARTESIAN_POINT('Ctrl Pts',(88.9647854578592,2.48656315467354,-2.77138752751406));
#9407=CARTESIAN_POINT('Ctrl Pts',(88.9502894328436,2.29025887611617,-2.9410860159636));
#9408=CARTESIAN_POINT('Ctrl Pts',(88.9392182292009,2.13655142010712,-3.05457143130824));
#9409=CARTESIAN_POINT('Ctrl Pts',(88.9180357866656,1.83159890814682,-3.24540697237114));
#9410=CARTESIAN_POINT('Ctrl Pts',(88.9079886350751,1.682418945424,-3.32519006561237));
#9411=CARTESIAN_POINT('Ctrl Pts',(88.8945741242445,1.47166198478017,-3.42007913692788));
#9412=CARTESIAN_POINT('Ctrl Pts',(88.8910027424847,1.41435753318342,-3.44417242865778));
#9413=CARTESIAN_POINT('Ctrl Pts',(88.8848047264691,1.31228714745151,-3.48410984953826));
#9414=CARTESIAN_POINT('Ctrl Pts',(88.8821550692265,1.26777128804404,-3.50055358015823));
#9415=CARTESIAN_POINT('Ctrl Pts',(88.8780552145461,1.19726655602733,-3.52507586705999));
#9416=CARTESIAN_POINT('Ctrl Pts',(88.8765760119042,1.17148390065933,-3.53372786667786));
#9417=CARTESIAN_POINT('Ctrl Pts',(88.8738542315812,1.12334177068792,-3.54929830729211));
#9418=CARTESIAN_POINT('Ctrl Pts',(88.8726075840097,1.10100773709355,-3.55628980999406));
#9419=CARTESIAN_POINT('Ctrl Pts',(88.8692014278906,1.03926167410361,-3.57498151166268));
#9420=CARTESIAN_POINT('Ctrl Pts',(88.8670651445378,0.999718354159187,-3.58624052655691));
#9421=CARTESIAN_POINT('Ctrl Pts',(88.8525579979586,0.726393416625571,-3.6591907873291));
#9422=CARTESIAN_POINT('Ctrl Pts',(88.8411322079086,0.48724908128512,-3.6986398726336));
#9423=CARTESIAN_POINT('Ctrl Pts',(88.8210452842138,0.0693639414856265,-3.72630851783919));
#9424=CARTESIAN_POINT('Ctrl Pts',(88.8124948751221,-0.107821275637139,-3.72539330121516));
#9425=CARTESIAN_POINT('Ctrl Pts',(88.7997846512026,-0.360040015419946,-3.70607812564811));
#9426=CARTESIAN_POINT('Ctrl Pts',(88.7959081711549,-0.435621180879112,-3.69795579998194));
#9427=CARTESIAN_POINT('Ctrl Pts',(88.7895152448493,-0.557590371981448,-3.68105726400317));
#9428=CARTESIAN_POINT('Ctrl Pts',(88.7870420336098,-0.604154334058376,-3.67370206767575));
#9429=CARTESIAN_POINT('Ctrl Pts',(88.7821702937406,-0.694576886866073,-3.65765342765294));
#9430=CARTESIAN_POINT('Ctrl Pts',(88.7797749241903,-0.738443381164276,-3.64905012144772));
#9431=CARTESIAN_POINT('Ctrl Pts',(88.7738538417917,-0.845372690050457,-3.62607159105905));
#9432=CARTESIAN_POINT('Ctrl Pts',(88.7703022616376,-0.908234575301005,-3.61083915777708));
#9433=CARTESIAN_POINT('Ctrl Pts',(88.751330180831,-1.23726325887303,-3.52197474243307));
#9434=CARTESIAN_POINT('Ctrl Pts',(88.7350463333981,-1.49499003332496,-3.42053958137388));
#9435=CARTESIAN_POINT('Ctrl Pts',(88.7095086293281,-1.87759794522472,-3.21838979981905));
#9436=CARTESIAN_POINT('Ctrl Pts',(88.7003075897857,-2.01135697332097,-3.13653573443043));
#9437=CARTESIAN_POINT('Ctrl Pts',(88.6888614998624,-2.17723465715658,-3.02003897546785));
#9438=CARTESIAN_POINT('Ctrl Pts',(88.6862943852759,-2.21440950985724,-2.9928877462384));
#9439=CARTESIAN_POINT('Ctrl Pts',(88.6822914701913,-2.27250748609849,-2.94877967154556));
#9440=CARTESIAN_POINT('Ctrl Pts',(88.6808287769051,-2.29376573649089,-2.93227397452747));
#9441=CARTESIAN_POINT('Ctrl Pts',(88.678113254031,-2.33333012967654,-2.90086112130445));
#9442=CARTESIAN_POINT('Ctrl Pts',(88.6768567906216,-2.35167696416519,-2.88600766708209));
#9443=CARTESIAN_POINT('Ctrl Pts',(88.6733829152909,-2.40246044310033,-2.84408789508451));
#9444=CARTESIAN_POINT('Ctrl Pts',(88.6711903289283,-2.43458033666695,-2.81664179577578));
#9445=CARTESIAN_POINT('Ctrl Pts',(88.6571449461076,-2.64003297376343,-2.63494376472635));
#9446=CARTESIAN_POINT('Ctrl Pts',(88.6461490978435,-2.79910533774633,-2.46530592000982));
#9447=CARTESIAN_POINT('Ctrl Pts',(88.6261107240962,-3.05530512538202,-2.13507240425678));
#9448=CARTESIAN_POINT('Ctrl Pts',(88.6171449357426,-3.15808570742325,-1.97987671932963));
#9449=CARTESIAN_POINT('Ctrl Pts',(88.6040144848518,-3.28559775587395,-1.75196526466524));
#9450=CARTESIAN_POINT('Ctrl Pts',(88.6001727315239,-3.3203516838051,-1.68517021365381));
#9451=CARTESIAN_POINT('Ctrl Pts',(88.5938204014959,-3.37349001454877,-1.5750063318007));
#9452=CARTESIAN_POINT('Ctrl Pts',(88.5913518523316,-3.39311916184391,-1.53226039442805));
#9453=CARTESIAN_POINT('Ctrl Pts',(88.5864775280323,-3.42986385083162,-1.44807145336529));
#9454=CARTESIAN_POINT('Ctrl Pts',(88.5840746532376,-3.44705101305148,-1.40666842158982));
#9455=CARTESIAN_POINT('Ctrl Pts',(88.5781118952671,-3.48742168811705,-1.30423126708377));
#9456=CARTESIAN_POINT('Ctrl Pts',(88.5745253651667,-3.50975468530323,-1.24287994488893));
#9457=CARTESIAN_POINT('Ctrl Pts',(88.5557650332944,-3.61661158733736,-0.923437066245195));
#9458=CARTESIAN_POINT('Ctrl Pts',(88.5397636267566,-3.67431166599015,-0.657275453897727));
#9459=CARTESIAN_POINT('Ctrl Pts',(88.5143435170982,-3.71911506418414,-0.228907073054607));
#9460=CARTESIAN_POINT('Ctrl Pts',(88.5049862263008,-3.72550271886407,-0.0696511161675265));
#9461=CARTESIAN_POINT('Ctrl Pts',(88.4933758970248,-3.72055898139491,0.135848430779211));
#9462=CARTESIAN_POINT('Ctrl Pts',(88.490791469862,-3.71858022525425,0.182141203561677));
#9463=CARTESIAN_POINT('Ctrl Pts',(88.4867673161267,-3.71408205582662,0.255324102884424));
#9464=CARTESIAN_POINT('Ctrl Pts',(88.485300298954,-3.71213344617649,0.282243301695779));
#9465=CARTESIAN_POINT('Ctrl Pts',(88.4824047992743,-3.70766088553837,0.33591714617746));
#9466=CARTESIAN_POINT('Ctrl Pts',(88.4809762930765,-3.70513965397643,0.362670369165699));
#9467=CARTESIAN_POINT('Ctrl Pts',(88.4771527425558,-3.69754054804012,0.434921969598884));
#9468=CARTESIAN_POINT('Ctrl Pts',(88.4747851438938,-3.6919126222383,0.480358999039255));
#9469=CARTESIAN_POINT('Ctrl Pts',(88.4598586819442,-3.65057995528813,0.770133492151917));
#9470=CARTESIAN_POINT('Ctrl Pts',(88.4482318779265,-3.59147432453225,1.01053211722554));
#9471=CARTESIAN_POINT('Ctrl Pts',(88.4276787042224,-3.44856265581029,1.41386695122147));
#9472=CARTESIAN_POINT('Ctrl Pts',(88.4188946236114,-3.37578581070706,1.57976808592928));
#9473=CARTESIAN_POINT('Ctrl Pts',(88.4063408879922,-3.25989249180027,1.79901880998709));
#9474=CARTESIAN_POINT('Ctrl Pts',(88.4028979724788,-3.22694718624467,1.85746571989442));
#9475=CARTESIAN_POINT('Ctrl Pts',(88.3970255296454,-3.16900466839523,1.95406062123651));
#9476=CARTESIAN_POINT('Ctrl Pts',(88.3946257685157,-3.14485266737148,1.9926979101459));
#9477=CARTESIAN_POINT('Ctrl Pts',(88.3900088785258,-3.09753828120153,2.06538596757483));
#9478=CARTESIAN_POINT('Ctrl Pts',(88.3877967640531,-3.07450805298463,2.09951486029721));
#9479=CARTESIAN_POINT('Ctrl Pts',(88.3818718100216,-3.01190688096473,2.18904521985672));
#9480=CARTESIAN_POINT('Ctrl Pts',(88.3781240189798,-2.97137548824645,2.24375331244069));
#9481=CARTESIAN_POINT('Ctrl Pts',(88.3656851753564,-2.8338933990256,2.41906028999436));
#9482=CARTESIAN_POINT('Ctrl Pts',(88.3567794841335,-2.73094174453057,2.53470751268217));
#9483=CARTESIAN_POINT('Ctrl Pts',(88.3477258692703,-2.62111999772913,2.64359556664866));
#9484=CARTESIAN_POINT('Ctrl Pts',(88.1029424533549,-2.62112001609809,2.64359554843587));
#9485=CARTESIAN_POINT('Ctrl Pts',(88.104827393899,-2.6446000911777,2.6203150981389));
#9486=CARTESIAN_POINT('Ctrl Pts',(88.1066980440785,-2.66777287808874,2.59671897917028));
#9487=CARTESIAN_POINT('Ctrl Pts',(88.110721425517,-2.71740373500025,2.54481533952543));
#9488=CARTESIAN_POINT('Ctrl Pts',(88.1128670494712,-2.74373799950446,2.51640024549215));
#9489=CARTESIAN_POINT('Ctrl Pts',(88.1163603226718,-2.78648353173111,2.46880813712911));
#9490=CARTESIAN_POINT('Ctrl Pts',(88.1177251218543,-2.80315154355,2.44986645501762));
#9491=CARTESIAN_POINT('Ctrl Pts',(88.1206139875581,-2.83838882781883,2.40899192472459));
#9492=CARTESIAN_POINT('Ctrl Pts',(88.1221341987369,-2.85689885897995,2.38701115277737));
#9493=CARTESIAN_POINT('Ctrl Pts',(88.1265554238813,-2.91054475537499,2.32178829339098));
#9494=CARTESIAN_POINT('Ctrl Pts',(88.1294123149259,-2.9449677254837,2.27796781038236));
#9495=CARTESIAN_POINT('Ctrl Pts',(88.1361650371508,-3.02522191071424,2.17094269986712));
#9496=CARTESIAN_POINT('Ctrl Pts',(88.1400167486146,-3.07007478313663,2.10703623624153));
#9497=CARTESIAN_POINT('Ctrl Pts',(88.1585229962119,-3.27831360160684,1.78955399165135));
#9498=CARTESIAN_POINT('Ctrl Pts',(88.172552382389,-3.41247338270368,1.51818168747295));
#9499=CARTESIAN_POINT('Ctrl Pts',(88.1917895691776,-3.53999809288119,1.1550781273012));
#9500=CARTESIAN_POINT('Ctrl Pts',(88.1960153612915,-3.564930464326,1.07566794129381));
#9501=CARTESIAN_POINT('Ctrl Pts',(88.202825832497,-3.60010339943074,0.948924974560949));
#9502=CARTESIAN_POINT('Ctrl Pts',(88.2053550649856,-3.6121180859515,0.902111825947858));
#9503=CARTESIAN_POINT('Ctrl Pts',(88.2102628935753,-3.63341547107911,0.811868670640676));
#9504=CARTESIAN_POINT('Ctrl Pts',(88.2126366141887,-3.64283907630651,0.768480293008751));
#9505=CARTESIAN_POINT('Ctrl Pts',(88.2183085894543,-3.66328839184387,0.665477462950102));
#9506=CARTESIAN_POINT('Ctrl Pts',(88.2216269655774,-3.67363809505849,0.605743066487205));
#9507=CARTESIAN_POINT('Ctrl Pts',(88.2354444802331,-3.71016812870533,0.359267300349725));
#9508=CARTESIAN_POINT('Ctrl Pts',(88.2463149520546,-3.72359845602328,0.170940362312663));
#9509=CARTESIAN_POINT('Ctrl Pts',(88.2724685176875,-3.72149562287613,-0.274500399021354));
#9510=CARTESIAN_POINT('Ctrl Pts',(88.2878736676169,-3.69368862339893,-0.530614676385393));
#9511=CARTESIAN_POINT('Ctrl Pts',(88.3048402312432,-3.6304675943449,-0.824934232501567));
#9512=CARTESIAN_POINT('Ctrl Pts',(88.3072951516026,-3.62044276122353,-0.867874407031743));
#9513=CARTESIAN_POINT('Ctrl Pts',(88.3111622734454,-3.60318582772701,-0.936279511793043));
#9514=CARTESIAN_POINT('Ctrl Pts',(88.3125986549176,-3.59644111070314,-0.961862193918668));
#9515=CARTESIAN_POINT('Ctrl Pts',(88.3154780346354,-3.58222108132513,-1.01355671691687));
#9516=CARTESIAN_POINT('Ctrl Pts',(88.3169202351315,-3.57473165532099,-1.03966281797688));
#9517=CARTESIAN_POINT('Ctrl Pts',(88.3208491473606,-3.55333701081578,-1.11127286053428));
#9518=CARTESIAN_POINT('Ctrl Pts',(88.3233055682666,-3.53884373647796,-1.15659702753469));
#9519=CARTESIAN_POINT('Ctrl Pts',(88.3289052048355,-3.50332677435404,-1.26074155644079));
#9520=CARTESIAN_POINT('Ctrl Pts',(88.3320222971041,-3.48168356566194,-1.31933617425825));
#9521=CARTESIAN_POINT('Ctrl Pts',(88.3435284448993,-3.3952900659898,-1.53627167913842));
#9522=CARTESIAN_POINT('Ctrl Pts',(88.3516544954185,-3.32112522513915,-1.69063810611603));
#9523=CARTESIAN_POINT('Ctrl Pts',(88.3688759871969,-3.14379534632403,-2.00267392944265));
#9524=CARTESIAN_POINT('Ctrl Pts',(88.3779696420024,-3.03876311178762,-2.15871799761719));
#9525=CARTESIAN_POINT('Ctrl Pts',(88.3909255993634,-2.88000925268686,-2.35989395274745));
#9526=CARTESIAN_POINT('Ctrl Pts',(88.3944347378501,-2.83613487198033,-2.41244502930289));
#9527=CARTESIAN_POINT('Ctrl Pts',(88.4003782403782,-2.76062702422136,-2.49797715936819));
#9528=CARTESIAN_POINT('Ctrl Pts',(88.4027807349994,-2.7297896093326,-2.53163976589444));
#9529=CARTESIAN_POINT('Ctrl Pts',(88.4076610982472,-2.66658071186967,-2.59814169273959));
#9530=CARTESIAN_POINT('Ctrl Pts',(88.4101390483007,-2.63420261666848,-2.63096356249864));
#9531=CARTESIAN_POINT('Ctrl Pts',(88.4164992171179,-2.55043293084138,-2.71278460780704));
#9532=CARTESIAN_POINT('Ctrl Pts',(88.4204159121678,-2.49823529902089,-2.76092881701725));
#9533=CARTESIAN_POINT('Ctrl Pts',(88.4292178137408,-2.37963729120204,-2.86419895946408));
#9534=CARTESIAN_POINT('Ctrl Pts',(88.4341277285961,-2.3126333094049,-2.91856729225456));
#9535=CARTESIAN_POINT('Ctrl Pts',(88.4515421286468,-2.07168127601554,-3.1005699659503));
#9536=CARTESIAN_POINT('Ctrl Pts',(88.464381802101,-1.88858947384899,-3.21537204128734));
#9537=CARTESIAN_POINT('Ctrl Pts',(88.4848148390558,-1.57904793569892,-3.37385799323009));
#9538=CARTESIAN_POINT('Ctrl Pts',(88.4924900246113,-1.4583614010496,-3.42775397885702));
#9539=CARTESIAN_POINT('Ctrl Pts',(88.502028059765,-1.29934536946942,-3.48884404558364));
#9540=CARTESIAN_POINT('Ctrl Pts',(88.5041459437752,-1.2634222934525,-3.50201306370316));
#9541=CARTESIAN_POINT('Ctrl Pts',(88.507607592847,-1.20355148370574,-3.52291984300524));
#9542=CARTESIAN_POINT('Ctrl Pts',(88.5089678672653,-1.17971740632928,-3.53097258094205));
#9543=CARTESIAN_POINT('Ctrl Pts',(88.5118627255322,-1.12829208302488,-3.54776860265111));
#9544=CARTESIAN_POINT('Ctrl Pts',(88.5133931338831,-1.10067756557123,-3.55643277509863));
#9545=CARTESIAN_POINT('Ctrl Pts',(88.5178810736388,-1.01855029465883,-3.5811523211024));
#9546=CARTESIAN_POINT('Ctrl Pts',(88.5207924273677,-0.963766057324589,-3.59628311808079));
#9547=CARTESIAN_POINT('Ctrl Pts',(88.5277085434199,-0.83076624075273,-3.62975837824628));
#9548=CARTESIAN_POINT('Ctrl Pts',(88.531666235363,-0.752260578365273,-3.64683747696754));
#9549=CARTESIAN_POINT('Ctrl Pts',(88.5430050657308,-0.523168863031586,-3.68896343098206));
#9550=CARTESIAN_POINT('Ctrl Pts',(88.5502556606628,-0.371519167082576,-3.70730796494108));
#9551=CARTESIAN_POINT('Ctrl Pts',(88.5659530603562,-0.0454642368930008,
-3.72653711703448));
#9552=CARTESIAN_POINT('Ctrl Pts',(88.5744104019956,0.128734914225388,-3.72458946953677));
#9553=CARTESIAN_POINT('Ctrl Pts',(88.5866464004245,0.369859855226244,-3.70495430767562));
#9554=CARTESIAN_POINT('Ctrl Pts',(88.5901305000481,0.437404254416894,-3.69758834042493));
#9555=CARTESIAN_POINT('Ctrl Pts',(88.595807138833,0.545341042563475,-3.68281858956291));
#9556=CARTESIAN_POINT('Ctrl Pts',(88.5979639292996,0.58587945749871,-3.67658737196949));
#9557=CARTESIAN_POINT('Ctrl Pts',(88.6025473616529,0.670976838102068,-3.66206380159366));
#9558=CARTESIAN_POINT('Ctrl Pts',(88.6049781783315,0.71550369373251,-3.65362497063357));
#9559=CARTESIAN_POINT('Ctrl Pts',(88.6110401221843,0.824998844997339,-3.63079487650112));
#9560=CARTESIAN_POINT('Ctrl Pts',(88.6146993266615,0.8897546904354,-3.61547097324373));
#9561=CARTESIAN_POINT('Ctrl Pts',(88.6283312126836,1.12605139098444,-3.5528207615217));
#9562=CARTESIAN_POINT('Ctrl Pts',(88.6386127284437,1.29453201990194,-3.49495381727692));
#9563=CARTESIAN_POINT('Ctrl Pts',(88.6639048739681,1.69070422161208,-3.32629440356851));
#9564=CARTESIAN_POINT('Ctrl Pts',(88.6790450116868,1.91251703535783,-3.20390408657019));
#9565=CARTESIAN_POINT('Ctrl Pts',(88.695824017371,2.15704541231188,-3.03447347045936));
#9566=CARTESIAN_POINT('Ctrl Pts',(88.6983197998562,2.19340366967098,-3.00829766516535));
#9567=CARTESIAN_POINT('Ctrl Pts',(88.702234949962,2.25058087167595,-2.96554557472101));
#9568=CARTESIAN_POINT('Ctrl Pts',(88.7036794952817,2.27170912181008,-2.94939190035971));
#9569=CARTESIAN_POINT('Ctrl Pts',(88.7065584232541,2.31392704295263,-2.91639119902499));
#9570=CARTESIAN_POINT('Ctrl Pts',(88.7079923220953,2.33501015366738,-2.89953852457337));
#9571=CARTESIAN_POINT('Ctrl Pts',(88.7118710237571,2.39211144376187,-2.85286813091862));
#9572=CARTESIAN_POINT('Ctrl Pts',(88.7142868069874,2.42775504930457,-2.82259801015629));
#9573=CARTESIAN_POINT('Ctrl Pts',(88.7250197460445,2.58577077741671,-2.68319567663285));
#9574=CARTESIAN_POINT('Ctrl Pts',(88.7329455114334,2.70143125993398,-2.56671523059201));
#9575=CARTESIAN_POINT('Ctrl Pts',(88.7534943810955,2.98233960389416,-2.24371496556524));
#9576=CARTESIAN_POINT('Ctrl Pts',(88.7660224629439,3.13393049565725,-2.02659235269491));
#9577=CARTESIAN_POINT('Ctrl Pts',(88.7827492310719,3.29315333297383,-1.737348313372));
#9578=CARTESIAN_POINT('Ctrl Pts',(88.7861443597917,3.3234843947264,-1.67859728600798));
#9579=CARTESIAN_POINT('Ctrl Pts',(88.7919284603268,3.37171604778075,-1.57873526970265));
#9580=CARTESIAN_POINT('Ctrl Pts',(88.7942884032278,3.3904677721366,-1.538051435188));
#9581=CARTESIAN_POINT('Ctrl Pts',(88.7991484089269,3.42717893766358,-1.45446698600369));
#9582=CARTESIAN_POINT('Ctrl Pts',(88.8016499525833,3.4450776820633,-1.41154850651784));
#9583=CARTESIAN_POINT('Ctrl Pts',(88.8081582148311,3.48907669736529,-1.30021974661874));
#9584=CARTESIAN_POINT('Ctrl Pts',(88.8122027366835,3.51397028608591,-1.23135673575019));
#9585=CARTESIAN_POINT('Ctrl Pts',(88.8213576283,3.56492768265269,-1.07623040719316));
#9586=CARTESIAN_POINT('Ctrl Pts',(88.8264961627339,3.58992217747943,-0.989665804135875));
#9587=CARTESIAN_POINT('Ctrl Pts',(88.8456145267138,3.67008303277628,-0.668790051456514));
#9588=CARTESIAN_POINT('Ctrl Pts',(88.860010743048,3.70563260448271,-0.430192759626316));
#9589=CARTESIAN_POINT('Ctrl Pts',(88.8800892350963,3.72318174986647,-0.0865362361471175));
#9590=CARTESIAN_POINT('Ctrl Pts',(88.8860444892711,3.72414901642061,0.0169684931800194));
#9591=CARTESIAN_POINT('Ctrl Pts',(88.8938416980841,3.71963348413003,0.156531915750616));
#9592=CARTESIAN_POINT('Ctrl Pts',(88.8958389585287,3.71793726594362,0.19266078435085));
#9593=CARTESIAN_POINT('Ctrl Pts',(88.8991786177201,3.71417079082982,0.253838948103428));
#9594=CARTESIAN_POINT('Ctrl Pts',(88.9005344810712,3.71237294848949,0.278901573804043));
#9595=CARTESIAN_POINT('Ctrl Pts',(88.903486058419,3.70786063795343,0.333984122159623));
#9596=CARTESIAN_POINT('Ctrl Pts',(88.9050761127884,3.70503518314193,0.363992187110998));
#9597=CARTESIAN_POINT('Ctrl Pts',(88.9099654414399,3.69512104083905,0.457149589248394));
#9598=CARTESIAN_POINT('Ctrl Pts',(88.9132053030085,3.68677953800527,0.520156453243628));
#9599=CARTESIAN_POINT('Ctrl Pts',(88.9211449827596,3.66198656661282,0.676540165080279));
#9600=CARTESIAN_POINT('Ctrl Pts',(88.9257770346585,3.64357360172728,0.769561717512575));
#9601=CARTESIAN_POINT('Ctrl Pts',(88.9453734479564,3.54975451915886,1.16383504216627));
#9602=CARTESIAN_POINT('Ctrl Pts',(88.9599042681047,3.44038240512592,1.45569059069758));
#9603=CARTESIAN_POINT('Ctrl Pts',(88.9789150292079,3.26628351775866,1.78727715231472));
#9604=CARTESIAN_POINT('Ctrl Pts',(88.9822089432988,3.23506071765283,1.84318994704575));
#9605=CARTESIAN_POINT('Ctrl Pts',(88.9878745966884,3.17973525009053,1.93652502756773));
#9606=CARTESIAN_POINT('Ctrl Pts',(88.9902202111532,3.15637478229152,1.97437166047396));
#9607=CARTESIAN_POINT('Ctrl Pts',(88.99509832939,3.10690779466692,2.05139141585444));
#9608=CARTESIAN_POINT('Ctrl Pts',(88.9976333096695,3.08072515318665,2.09050593012863));
#9609=CARTESIAN_POINT('Ctrl Pts',(89.0043458539657,3.01020054116036,2.19166013839208));
#9610=CARTESIAN_POINT('Ctrl Pts',(89.0085659127104,2.96468332354661,2.25284999896869));
#9611=CARTESIAN_POINT('Ctrl Pts',(89.0235158806796,2.79941859606333,2.46133011291959));
#9612=CARTESIAN_POINT('Ctrl Pts',(89.034576293122,2.67032539840791,2.60081519371446));
#9613=CARTESIAN_POINT('Ctrl Pts',(89.0590032766803,2.36650822081009,2.8825221331891));
#9614=CARTESIAN_POINT('Ctrl Pts',(89.0723763774385,2.1883564808912,3.02000017347433));
#9615=CARTESIAN_POINT('Ctrl Pts',(89.0874414131702,1.96260541531723,3.16368421629125));
#9616=CARTESIAN_POINT('Ctrl Pts',(89.0898341150602,1.92591810365992,3.18615090749703));
#9617=CARTESIAN_POINT('Ctrl Pts',(89.0936282618884,1.8662304856135,3.22129480869734));
#9618=CARTESIAN_POINT('Ctrl Pts',(89.0950523829701,1.84347166086447,3.23437301885312));
#9619=CARTESIAN_POINT('Ctrl Pts',(89.0979325178397,1.79666417301898,3.2606160276992));
#9620=CARTESIAN_POINT('Ctrl Pts',(89.0993872465129,1.77260487817393,3.27375794271531));
#9621=CARTESIAN_POINT('Ctrl Pts',(89.1033959931179,1.70522978174943,3.30959971015756));
#9622=CARTESIAN_POINT('Ctrl Pts',(89.1059175916601,1.66160741121389,3.33171428596256));
#9623=CARTESIAN_POINT('Ctrl Pts',(89.1116999232661,1.55912040002446,3.38115678139712));
#9624=CARTESIAN_POINT('Ctrl Pts',(89.1149319801386,1.49995111951618,3.407818207222));
#9625=CARTESIAN_POINT('Ctrl Pts',(89.1272487532407,1.26898963496278,3.50470673823234));
#9626=CARTESIAN_POINT('Ctrl Pts',(89.136032872342,1.09273259043286,3.5635999609455));
#9627=CARTESIAN_POINT('Ctrl Pts',(89.1539140185139,0.732213255348467,3.65478236498869));
#9628=CARTESIAN_POINT('Ctrl Pts',(89.1629903293211,0.548451413037632,3.68683645613083));
#9629=CARTESIAN_POINT('Ctrl Pts',(89.1755625381924,0.30278680742791,3.71091057225073));
#9630=CARTESIAN_POINT('Ctrl Pts',(89.1786876059433,0.242365807597258,3.7153459350924));
#9631=CARTESIAN_POINT('Ctrl Pts',(89.1841789574466,0.137544976599814,3.72047281307354));
#9632=CARTESIAN_POINT('Ctrl Pts',(89.1865241510833,0.093190541973855,3.72184791111675));
#9633=CARTESIAN_POINT('Ctrl Pts',(89.1914729873382,0.000523619055112301,
3.72306332900135));
#9634=CARTESIAN_POINT('Ctrl Pts',(89.1940806467488,-0.0477822142588712,
3.72275669244417));
#9635=CARTESIAN_POINT('Ctrl Pts',(89.2012555985288,-0.179211715953318,3.71936397562102));
#9636=CARTESIAN_POINT('Ctrl Pts',(89.20587696523,-0.262256342258192,3.71443203923228));
#9637=CARTESIAN_POINT('Ctrl Pts',(89.2166851209834,-0.452840211623173,3.6966904263104));
#9638=CARTESIAN_POINT('Ctrl Pts',(89.2229194763831,-0.560122945145468,3.68196198506632));
#9639=CARTESIAN_POINT('Ctrl Pts',(89.2385841869463,-0.824299585553218,3.63388068176301));
#9640=CARTESIAN_POINT('Ctrl Pts',(89.248098923262,-0.979972456563201,3.59502574567587));
#9641=CARTESIAN_POINT('Ctrl Pts',(89.2658772279148,-1.26773401371308,3.50311675968315));
#9642=CARTESIAN_POINT('Ctrl Pts',(89.2741419269388,-1.40025266201107,3.452285484909));
#9643=CARTESIAN_POINT('Ctrl Pts',(89.2842505168112,-1.56476492097124,3.3781459027993));
#9644=CARTESIAN_POINT('Ctrl Pts',(89.2863893941991,-1.59972614212561,3.36173102746785));
#9645=CARTESIAN_POINT('Ctrl Pts',(89.2898742818897,-1.65706668010135,3.33371152441502));
#9646=CARTESIAN_POINT('Ctrl Pts',(89.2912373073047,-1.67959440904065,3.32241858652376));
#9647=CARTESIAN_POINT('Ctrl Pts',(89.2941248181073,-1.72757054124143,3.29775586739967));
#9648=CARTESIAN_POINT('Ctrl Pts',(89.295645401778,-1.7529816170667,3.2843186947899));
#9649=CARTESIAN_POINT('Ctrl Pts',(89.3000726332398,-1.82728089756894,3.24392180068835));
#9650=CARTESIAN_POINT('Ctrl Pts',(89.3029349038935,-1.87572286928738,3.21615429447506));
#9651=CARTESIAN_POINT('Ctrl Pts',(89.3097037222228,-1.99054620475305,3.14685896049157));
#9652=CARTESIAN_POINT('Ctrl Pts',(89.3135658043411,-2.05627880024351,3.10430573145286));
#9653=CARTESIAN_POINT('Ctrl Pts',(89.3279815533104,-2.29942167297044,2.93578829575765));
#9654=CARTESIAN_POINT('Ctrl Pts',(89.3382058393382,-2.46687344235342,2.79653073526865));
#9655=CARTESIAN_POINT('Ctrl Pts',(89.3487674494621,-2.62112000711955,2.64359555733807));
#9656=CARTESIAN_POINT('Origin',(80.1322559480305,0.,0.));
#9657=CARTESIAN_POINT('',(89.5089317511108,-3.72371574749209,0.00232684839586724));
#9658=CARTESIAN_POINT('Ctrl Pts',(89.3487674494621,-2.62112000711955,2.64359555733807));
#9659=CARTESIAN_POINT('Ctrl Pts',(89.3529797741928,-2.68263871608259,2.58259987347577));
#9660=CARTESIAN_POINT('Ctrl Pts',(89.3572420136609,-2.74205702040921,2.51942838131009));
#9661=CARTESIAN_POINT('Ctrl Pts',(89.3656756632406,-2.853179327034,2.39268167386431));
#9662=CARTESIAN_POINT('Ctrl Pts',(89.369832700608,-2.90505703882765,2.32942058856126));
#9663=CARTESIAN_POINT('Ctrl Pts',(89.3765592883275,-2.98404385599776,2.22635576065072));
#9664=CARTESIAN_POINT('Ctrl Pts',(89.3790758305599,-3.01253811375682,2.18764520527887));
#9665=CARTESIAN_POINT('Ctrl Pts',(89.3839757636083,-3.06594189295966,2.11207151816034));
#9666=CARTESIAN_POINT('Ctrl Pts',(89.3863546743921,-3.09095586216386,2.07529212844363));
#9667=CARTESIAN_POINT('Ctrl Pts',(89.3920672311352,-3.14883459893498,1.98682142883577));
#9668=CARTESIAN_POINT('Ctrl Pts',(89.395421829218,-3.18109364008708,1.93475098583921));
#9669=CARTESIAN_POINT('Ctrl Pts',(89.4100519670901,-3.31437529037645,1.70726532986437));
#9670=CARTESIAN_POINT('Ctrl Pts',(89.4217623866582,-3.40227226634272,1.52458661664443));
#9671=CARTESIAN_POINT('Ctrl Pts',(89.4479525859899,-3.56198134792401,1.10909395211884));
#9672=CARTESIAN_POINT('Ctrl Pts',(89.4624645439403,-3.62671150748733,0.874513249080568));
#9673=CARTESIAN_POINT('Ctrl Pts',(89.4785770302165,-3.67553767807969,0.592594548908786));
#9674=CARTESIAN_POINT('Ctrl Pts',(89.4809882160038,-3.68218712340376,0.54976706659954));
#9675=CARTESIAN_POINT('Ctrl Pts',(89.4848047716062,-3.69167116223613,0.480754062023185));
#9676=CARTESIAN_POINT('Ctrl Pts',(89.4862332372311,-3.69497830122412,0.45463822564063));
#9677=CARTESIAN_POINT('Ctrl Pts',(89.4888859989603,-3.70066628243186,0.405548898349816));
#9678=CARTESIAN_POINT('Ctrl Pts',(89.4901139226997,-3.70311083491576,0.382584686000311));
#9679=CARTESIAN_POINT('Ctrl Pts',(89.4928019861062,-3.70803668507492,0.331828214641216));
#9680=CARTESIAN_POINT('Ctrl Pts',(89.4942571729711,-3.71041956024529,0.304027619698432));
#9681=CARTESIAN_POINT('Ctrl Pts',(89.5004197418618,-3.71926890458101,0.18508175469496));
#9682=CARTESIAN_POINT('Ctrl Pts',(89.5049934840879,-3.72269148191928,0.0937369082323972));
#9683=CARTESIAN_POINT('Ctrl Pts',(89.5094878198556,-3.72274925601168,0.00235358545693844));
#9684=CARTESIAN_POINT('',(90.4429666115571,0.0630273376275202,3.72323065059699));
#9685=CARTESIAN_POINT('Ctrl Pts',(89.5089317511109,-3.72371574749208,0.0023268483958672));
#9686=CARTESIAN_POINT('Ctrl Pts',(89.5144493688092,-3.72357263772784,-0.107412055256537));
#9687=CARTESIAN_POINT('Ctrl Pts',(89.5198863329416,-3.71852748988571,-0.217314149425214));
#9688=CARTESIAN_POINT('Ctrl Pts',(89.5253164743333,-3.70860419682644,-0.326901558437555));
#9689=CARTESIAN_POINT('Ctrl Pts',(89.530740622285,-3.69869185645852,-0.436368011930497));
#9690=CARTESIAN_POINT('Ctrl Pts',(89.5361583414371,-3.68391252706447,-0.545520371229198));
#9691=CARTESIAN_POINT('Ctrl Pts',(89.5416289472312,-3.66433387024312,-0.653894300217409));
#9692=CARTESIAN_POINT('Ctrl Pts',(89.547095047411,-3.64477133848699,-0.762178971975731));
#9693=CARTESIAN_POINT('Ctrl Pts',(89.5526141925419,-3.62041766047029,-0.869686450491287));
#9694=CARTESIAN_POINT('Ctrl Pts',(89.558226648156,-3.59137910554205,-0.975966541823195));
#9695=CARTESIAN_POINT('Ctrl Pts',(89.5638366528022,-3.56235323179511,-1.08220022047689));
#9696=CARTESIAN_POINT('Ctrl Pts',(89.5695400284607,-3.5286467523647,-1.18720755362765));
#9697=CARTESIAN_POINT('Ctrl Pts',(89.5753552132139,-3.4904011333468,-1.29055246128007));
#9698=CARTESIAN_POINT('Ctrl Pts',(89.5811693810291,-3.4521622025814,-1.393879296357));
#9699=CARTESIAN_POINT('Ctrl Pts',(89.5870953775833,-3.40938581625973,-1.49554425436715));
#9700=CARTESIAN_POINT('Ctrl Pts',(89.5931283660254,-3.3622466314541,-1.59512547099244));
#9701=CARTESIAN_POINT('Ctrl Pts',(89.5991618790538,-3.3151033477561,-1.6947153465008));
#9702=CARTESIAN_POINT('Ctrl Pts',(89.6053023841074,-3.26359652083738,-1.79222107456204));
#9703=CARTESIAN_POINT('Ctrl Pts',(89.6115214661064,-3.20793329375971,-1.88723523931771));
#9704=CARTESIAN_POINT('Ctrl Pts',(89.6177464373095,-3.15221735599179,-1.98233937841498));
#9705=CARTESIAN_POINT('Ctrl Pts',(89.6240500301323,-3.0923370587168,-2.07494716306154));
#9706=CARTESIAN_POINT('Ctrl Pts',(89.6303810247902,-3.02853314866813,-2.16466544028031));
#9707=CARTESIAN_POINT('Ctrl Pts',(89.6367151237953,-2.96469795293667,-2.25442771006255));
#9708=CARTESIAN_POINT('Ctrl Pts',(89.64307642923,-2.89693510650364,-2.34129751029344));
#9709=CARTESIAN_POINT('Ctrl Pts',(89.6493933299385,-2.82552077623839,-2.42489797482477));
#9710=CARTESIAN_POINT('Ctrl Pts',(89.6557200436836,-2.75399550684918,-2.50862830912122));
#9711=CARTESIAN_POINT('Ctrl Pts',(89.6620018381212,-2.67880709980692,-2.58907888684311));
#9712=CARTESIAN_POINT('Ctrl Pts',(89.6681508424376,-2.60027188408617,-2.66589079960463));
#9713=CARTESIAN_POINT('Ctrl Pts',(89.6728964356274,-2.53966106553649,-2.72517163131961));
#9714=CARTESIAN_POINT('Ctrl Pts',(89.6775625153991,-2.477057541777,-2.78228549830324));
#9715=CARTESIAN_POINT('Ctrl Pts',(89.6821048509549,-2.41262437404084,-2.83707738434133));
#9716=CARTESIAN_POINT('Ctrl Pts',(89.6821072920214,-2.41258974743762,-2.83710682968702));
#9717=CARTESIAN_POINT('Ctrl Pts',(89.6821097330548,-2.4125551202594,-2.83713627440416));
#9718=CARTESIAN_POINT('Ctrl Pts',(89.6821121740549,-2.41252049250622,-2.8371657184927));
#9719=CARTESIAN_POINT('Ctrl Pts',(89.6874488481156,-2.33681503472848,-2.90153830975086));
#9720=CARTESIAN_POINT('Ctrl Pts',(89.6926267789551,-2.25835696697216,-2.96290651400831));
#9721=CARTESIAN_POINT('Ctrl Pts',(89.6977083378158,-2.17743387421516,-3.0210494835982));
#9722=CARTESIAN_POINT('Ctrl Pts',(89.6982961279809,-2.16807340051844,-3.02777495242241));
#9723=CARTESIAN_POINT('Ctrl Pts',(89.6988826287051,-2.15868000253057,-3.03445726790254));
#9724=CARTESIAN_POINT('Ctrl Pts',(89.6994679365177,-2.1492541702095,-3.04109608898255));
#9725=CARTESIAN_POINT('Ctrl Pts',(89.7051084814648,-2.05841849414079,-3.10507365409939));
#9726=CARTESIAN_POINT('Ctrl Pts',(89.7106388626614,-1.96456457426539,-3.16501220907957));
#9727=CARTESIAN_POINT('Ctrl Pts',(89.7161398493902,-1.86811509933513,-3.22065648999706));
#9728=CARTESIAN_POINT('Ctrl Pts',(89.7216353495229,-1.7717618215652,-3.27624527220066));
#9729=CARTESIAN_POINT('Ctrl Pts',(89.7271019533148,-1.67281850372914,-3.32754867921573));
#9730=CARTESIAN_POINT('Ctrl Pts',(89.732606643235,-1.57172006659594,-3.37435762076696));
#9731=CARTESIAN_POINT('Ctrl Pts',(89.7381075151489,-1.47069175048162,-3.42113409603317));
#9732=CARTESIAN_POINT('Ctrl Pts',(89.7436467064045,-1.36751150125765,-3.4634226070263));
#9733=CARTESIAN_POINT('Ctrl Pts',(89.7492721239457,-1.26262286082101,-3.50105529733182));
#9734=CARTESIAN_POINT('Ctrl Pts',(89.7548954830333,-1.15777260124904,-3.53867421707851));
#9735=CARTESIAN_POINT('Ctrl Pts',(89.760605173825,-1.05121531499535,-3.5716409057542));
#9736=CARTESIAN_POINT('Ctrl Pts',(89.7664267450917,-0.943401282902844,-3.59982509011847));
#9737=CARTESIAN_POINT('Ctrl Pts',(89.7722476261605,-0.835600033102613,-3.62800593300228));
#9738=CARTESIAN_POINT('Ctrl Pts',(89.7781804392221,-0.726542398257346,-3.65140550588009));
#9739=CARTESIAN_POINT('Ctrl Pts',(89.7842265888405,-0.616684413474052,-3.66992886131566));
#9740=CARTESIAN_POINT('Ctrl Pts',(89.7902735172042,-0.506812278960044,-3.68845460256317));
#9741=CARTESIAN_POINT('Ctrl Pts',(89.7964338106735,-0.396139610282474,-3.70210288836393));
#9742=CARTESIAN_POINT('Ctrl Pts',(89.8026841522676,-0.285127903742074,-3.71081313279568));
#9743=CARTESIAN_POINT('Ctrl Pts',(89.8089408354159,-0.174003565477832,-3.71953221458231));
#9744=CARTESIAN_POINT('Ctrl Pts',(89.8152876659514,-0.0625394855586726,
-3.72330314762807));
#9745=CARTESIAN_POINT('Ctrl Pts',(89.8216770954455,0.0487961803852812,-3.72210009108173));
#9746=CARTESIAN_POINT('Ctrl Pts',(89.8280697237272,0.160187585132733,-3.72089643224024));
#9747=CARTESIAN_POINT('Ctrl Pts',(89.8345047957465,0.271450483496589,-3.7147135964053));
#9748=CARTESIAN_POINT('Ctrl Pts',(89.8409126010786,0.38211034631084,-3.70356277017798));
#9749=CARTESIAN_POINT('Ctrl Pts',(89.8473309919939,0.492953017297544,-3.69239352297929));
#9750=CARTESIAN_POINT('Ctrl Pts',(89.8537216764366,0.603190667762472,-3.67623947787963));
#9751=CARTESIAN_POINT('Ctrl Pts',(89.8599964980888,0.712340311951511,-3.65515343115013));
#9752=CARTESIAN_POINT('Ctrl Pts',(89.8657030852584,0.81160559686597,-3.63597689189637));
#9753=CARTESIAN_POINT('Ctrl Pts',(89.871313353658,0.909971355674651,-3.61272118873168));
#9754=CARTESIAN_POINT('Ctrl Pts',(89.8767525586254,1.00706894884951,-3.58546115444386));
#9755=CARTESIAN_POINT('Ctrl Pts',(89.8770619556114,1.01259212785528,-3.58391052847928));
#9756=CARTESIAN_POINT('Ctrl Pts',(89.8773707990964,1.01811121649432,-3.58234695125233));
#9757=CARTESIAN_POINT('Ctrl Pts',(89.8776790753233,1.02362615165207,-3.5807704383915));
#9758=CARTESIAN_POINT('Ctrl Pts',(89.8776815122706,1.02366974763763,-3.58075797593638));
#9759=CARTESIAN_POINT('Ctrl Pts',(89.8776839491846,1.02371334341927,-3.58074551265842));
#9760=CARTESIAN_POINT('Ctrl Pts',(89.8776863860656,1.02375693899699,-3.58073304855759));
#9761=CARTESIAN_POINT('Ctrl Pts',(89.8830296183515,1.11934687701787,-3.55340361085902));
#9762=CARTESIAN_POINT('Ctrl Pts',(89.8882135303408,1.21395884304279,-3.52211453451959));
#9763=CARTESIAN_POINT('Ctrl Pts',(89.8933001623114,1.3072499547986,-3.4869829616927));
#9764=CARTESIAN_POINT('Ctrl Pts',(89.8938972847919,1.31820144890839,-3.48285884734097));
#9765=CARTESIAN_POINT('Ctrl Pts',(89.8944930667014,1.32913470820646,-3.4786818304396));
#9766=CARTESIAN_POINT('Ctrl Pts',(89.8950876084025,1.34004915277909,-3.47445214012305));
#9767=CARTESIAN_POINT('Ctrl Pts',(89.900741891935,1.44384904451091,-3.43422641961143));
#9768=CARTESIAN_POINT('Ctrl Pts',(89.9062846299621,1.545950830139,-3.38923164780696));
#9769=CARTESIAN_POINT('Ctrl Pts',(89.9117967189255,1.64590618376087,-3.33967935958924));
#9770=CARTESIAN_POINT('Ctrl Pts',(89.9173032706963,1.74576112680444,-3.29017684933473));
#9771=CARTESIAN_POINT('Ctrl Pts',(89.9227796787904,1.84347404259024,-3.23612644845506));
#9772=CARTESIAN_POINT('Ctrl Pts',(89.9282931675701,1.93862843278367,-3.17777550341602));
#9773=CARTESIAN_POINT('Ctrl Pts',(89.9338027148404,2.03371479854958,-3.11946627258085));
#9774=CARTESIAN_POINT('Ctrl Pts',(89.9393495788318,2.12624641327672,-3.05686295954206));
#9775=CARTESIAN_POINT('Ctrl Pts',(89.9449819661159,2.21583646266807,-2.99024292319167));
#9776=CARTESIAN_POINT('Ctrl Pts',(89.9506122147042,2.30539249347191,-2.92364818339543));
#9777=CARTESIAN_POINT('Ctrl Pts',(89.9563280920228,2.39200928482382,-2.85303996676748));
#9778=CARTESIAN_POINT('Ctrl Pts',(89.9621554707194,2.47532764309845,-2.77872204621894));
#9779=CARTESIAN_POINT('Ctrl Pts',(89.9679820610267,2.55863472918569,-2.70441418018354));
#9780=CARTESIAN_POINT('Ctrl Pts',(89.9739202015018,2.63864432622805,-2.62639772042333));
#9781=CARTESIAN_POINT('Ctrl Pts',(89.9799716257893,2.71502347934517,-2.54500079096971));
#9782=CARTESIAN_POINT('Ctrl Pts',(89.9860237104523,2.79141096751009,-2.4635949788921));
#9783=CARTESIAN_POINT('Ctrl Pts',(89.9921891031505,2.86416722408592,-2.3788079853391));
#9784=CARTESIAN_POINT('Ctrl Pts',(89.9984448156139,2.93298485751985,-2.29099153144459));
#9785=CARTESIAN_POINT('Ctrl Pts',(90.0047065906403,3.00186918379431,-2.20308997249105));
#9786=CARTESIAN_POINT('Ctrl Pts',(90.0110587764147,3.06680718997094,-2.11215301755072));
#9787=CARTESIAN_POINT('Ctrl Pts',(90.0174541626742,3.12751670253634,-2.01855720431008));
#9788=CARTESIAN_POINT('Ctrl Pts',(90.0238526125877,3.18825529746403,-1.92491655481174));
#9789=CARTESIAN_POINT('Ctrl Pts',(90.030294105395,3.24476119420331,-1.82861435236295));
#9790=CARTESIAN_POINT('Ctrl Pts',(90.0367092909392,3.29677947739771,-1.7300530380692));
#9791=CARTESIAN_POINT('Ctrl Pts',(90.043134691733,3.34888059214043,-1.63133477922123));
#9792=CARTESIAN_POINT('Ctrl Pts',(90.0495333501238,3.39647947670092,-1.53034998886078));
#9793=CARTESIAN_POINT('Ctrl Pts',(90.0558175263701,3.43935117920548,-1.4275312671387));
#9794=CARTESIAN_POINT('Ctrl Pts',(90.0617137179113,3.47957598509268,-1.33106056779102));
#9795=CARTESIAN_POINT('Ctrl Pts',(90.0675085846285,3.51563920871451,-1.2329755145455));
#9796=CARTESIAN_POINT('Ctrl Pts',(90.0731205045349,3.54738485993372,-1.1336585668842));
#9797=CARTESIAN_POINT('Ctrl Pts',(90.0731228130997,3.54739791908159,-1.13361771106126));
#9798=CARTESIAN_POINT('Ctrl Pts',(90.0731251216355,3.5474109775156,-1.13357685498283));
#9799=CARTESIAN_POINT('Ctrl Pts',(90.0731274301423,3.5474240352357,-1.13353599864897));
#9800=CARTESIAN_POINT('Ctrl Pts',(90.0785089336928,3.57786369706669,-1.03829326282715));
#9801=CARTESIAN_POINT('Ctrl Pts',(90.0837330158939,3.60442229610753,-0.941658259288835));
#9802=CARTESIAN_POINT('Ctrl Pts',(90.0888624878585,3.62700700971911,-0.843986516594742));
#9803=CARTESIAN_POINT('Ctrl Pts',(90.0894422182873,3.62955952307635,-0.832947703699474));
#9804=CARTESIAN_POINT('Ctrl Pts',(90.0900207402207,3.63206129679853,-0.82189569892181));
#9805=CARTESIAN_POINT('Ctrl Pts',(90.0905981443356,3.63451221327311,-0.810831053933906));
#9806=CARTESIAN_POINT('Ctrl Pts',(90.0962795442613,3.65862814233822,-0.701959863738108));
#9807=CARTESIAN_POINT('Ctrl Pts',(90.1018533394814,3.67781824642278,-0.591859185322982));
#9808=CARTESIAN_POINT('Ctrl Pts',(90.107399858104,3.69201071129179,-0.481020504528848));
#9809=CARTESIAN_POINT('Ctrl Pts',(90.112940950973,3.7061892927104,-0.370290249109893));
#9810=CARTESIAN_POINT('Ctrl Pts',(90.1184552562561,3.71538045084791,-0.258823609572112));
#9811=CARTESIAN_POINT('Ctrl Pts',(90.1240089386278,3.71955946056852,-0.147105405430518));
#9812=CARTESIAN_POINT('Ctrl Pts',(90.1295588275376,3.72373561580207,-0.0354635107954085));
#9813=CARTESIAN_POINT('Ctrl Pts',(90.1351483217634,3.72290679006134,0.0764295340686877));
#9814=CARTESIAN_POINT('Ctrl Pts',(90.140824191506,3.71708940717279,0.188096888452428));
#9815=CARTESIAN_POINT('Ctrl Pts',(90.1464980116806,3.71127412495294,0.299723919529344));
#9816=CARTESIAN_POINT('Ctrl Pts',(90.1522583096122,3.70047409704029,0.411125395761373));
#9817=CARTESIAN_POINT('Ctrl Pts',(90.1581292358594,3.68474284199021,0.521832672354837));
#9818=CARTESIAN_POINT('Ctrl Pts',(90.1639994626508,3.66901346114476,0.632526759403664));
#9819=CARTESIAN_POINT('Ctrl Pts',(90.1699803652306,3.64835413879587,0.742526800876524));
#9820=CARTESIAN_POINT('Ctrl Pts',(90.1760717472594,3.62285309736902,0.851372273936879));
#9821=CARTESIAN_POINT('Ctrl Pts',(90.1821638774131,3.59734892398235,0.960231115064904));
#9822=CARTESIAN_POINT('Ctrl Pts',(90.1883665079535,3.56700185768382,1.06793509862119));
#9823=CARTESIAN_POINT('Ctrl Pts',(90.1946545894918,3.53193393770647,1.17403160929122));
#9824=CARTESIAN_POINT('Ctrl Pts',(90.2009488270132,3.49683168650664,1.28023198762478));
#9825=CARTESIAN_POINT('Ctrl Pts',(90.2073285908265,3.45699923761497,1.38482173281706));
#9826=CARTESIAN_POINT('Ctrl Pts',(90.2137445723081,3.41259342922832,1.48735510350216));
#9827=CARTESIAN_POINT('Ctrl Pts',(90.2201636768321,3.36816600587628,1.58993838331716));
#9828=CARTESIAN_POINT('Ctrl Pts',(90.2266188231901,3.31916054605349,1.69046324136125));
#9829=CARTESIAN_POINT('Ctrl Pts',(90.233038676517,3.26577094640859,1.78849187087495));
#9830=CARTESIAN_POINT('Ctrl Pts',(90.239468716635,3.2122966300783,1.88667604867183));
#9831=CARTESIAN_POINT('Ctrl Pts',(90.2458629821864,3.15442387293282,1.98235592320623));
#9832=CARTESIAN_POINT('Ctrl Pts',(90.2521320849717,3.09238895186967,2.07510156630849));
#9833=CARTESIAN_POINT('Ctrl Pts',(90.2579064984125,3.03524915144765,2.16052873291163));
#9834=CARTESIAN_POINT('Ctrl Pts',(90.263574174664,2.97457828973752,2.24346635863138));
#9835=CARTESIAN_POINT('Ctrl Pts',(90.2690571354595,2.91059682083417,2.32358854504316));
#9836=CARTESIAN_POINT('Ctrl Pts',(90.2690597464048,2.91056635333286,2.32362669863453));
#9837=CARTESIAN_POINT('Ctrl Pts',(90.2690623573112,2.91053588503632,2.32366485164704));
#9838=CARTESIAN_POINT('Ctrl Pts',(90.2690649681786,2.91050541594457,2.32370300408063));
#9839=CARTESIAN_POINT('Ctrl Pts',(90.2742912628997,2.84951401777874,2.40007450498025));
#9840=CARTESIAN_POINT('Ctrl Pts',(90.279361515835,2.78533191663936,2.47412713275621));
#9841=CARTESIAN_POINT('Ctrl Pts',(90.2843364642347,2.71818833114402,2.54559156128984));
#9842=CARTESIAN_POINT('Ctrl Pts',(90.2848916878766,2.71069484516782,2.55356727019879));
#9843=CARTESIAN_POINT('Ctrl Pts',(90.2854457244594,2.70316452526199,2.56151073285841));
#9844=CARTESIAN_POINT('Ctrl Pts',(90.2859986584125,2.69559772974738,2.56942156881173));
#9845=CARTESIAN_POINT('Ctrl Pts',(90.2915013907409,2.62029388909111,2.648149258616));
#9846=CARTESIAN_POINT('Ctrl Pts',(90.2968955092956,2.54137164504299,2.7236468238917));
#9847=CARTESIAN_POINT('Ctrl Pts',(90.3022592981764,2.45917985900135,2.79558902582741));
#9848=CARTESIAN_POINT('Ctrl Pts',(90.3076891130458,2.37597632658979,2.86841680605698));
#9849=CARTESIAN_POINT('Ctrl Pts',(90.313088318592,2.2894226369102,2.93760128305359));
#9850=CARTESIAN_POINT('Ctrl Pts',(90.3185249978489,2.19990511535511,3.00284842676939));
#9851=CARTESIAN_POINT('Ctrl Pts',(90.3238866980851,2.11162215919905,3.06719572579984));
#9852=CARTESIAN_POINT('Ctrl Pts',(90.3292850898537,2.02045687391114,3.12771381930532));
#9853=CARTESIAN_POINT('Ctrl Pts',(90.3347675827141,1.92679819254861,3.1841592531776));
#9854=CARTESIAN_POINT('Ctrl Pts',(90.3402483626254,1.83316877388635,3.24058705124945));
#9855=CARTESIAN_POINT('Ctrl Pts',(90.3458133571018,1.73704769886038,3.2929448632473));
#9856=CARTESIAN_POINT('Ctrl Pts',(90.3514888410463,1.63883842014456,3.34102540163832));
#9857=CARTESIAN_POINT('Ctrl Pts',(90.3571640816788,1.54063335172977,3.38910387878275));
#9858=CARTESIAN_POINT('Ctrl Pts',(90.3629498814715,1.44034038203927,3.43290551935315));
#9859=CARTESIAN_POINT('Ctrl Pts',(90.3688495987068,1.33837552613422,3.47225751229601));
#9860=CARTESIAN_POINT('Ctrl Pts',(90.3748968291848,1.23386119777986,3.51259344054621));
#9861=CARTESIAN_POINT('Ctrl Pts',(90.3810638525647,1.12759036442714,3.54825428961313));
#9862=CARTESIAN_POINT('Ctrl Pts',(90.3873286302831,1.02002315918263,3.57909084133929));
#9863=CARTESIAN_POINT('Ctrl Pts',(90.3934482336772,0.914948619605076,3.60921281455055));
#9864=CARTESIAN_POINT('Ctrl Pts',(90.3996609409719,0.808637163127249,3.63473156593701));
#9865=CARTESIAN_POINT('Ctrl Pts',(90.4059228398357,0.701528198865719,3.65554273541497));
#9866=CARTESIAN_POINT('Ctrl Pts',(90.412407563663,0.590607842630952,3.67709445471385));
#9867=CARTESIAN_POINT('Ctrl Pts',(90.4189449773761,0.478832125313426,3.69359719226042));
#9868=CARTESIAN_POINT('Ctrl Pts',(90.4254623811125,0.366700747059007,3.70497562314993));
#9869=CARTESIAN_POINT('Ctrl Pts',(90.4313363109118,0.265640283290959,3.71523064293606));
#9870=CARTESIAN_POINT('Ctrl Pts',(90.4371936819014,0.16429017486761,3.72132334342145));
#9871=CARTESIAN_POINT('Ctrl Pts',(90.4429666115571,0.06302733762752,3.72323065059699));
#9872=CARTESIAN_POINT('',(90.4430005297901,3.5302572329849,1.18158852036477));
#9873=CARTESIAN_POINT('Origin',(90.4430005297901,0.,0.));
#9874=CARTESIAN_POINT('',(89.755930604391,-3.72148643608346,0.000620124237849482));
#9875=CARTESIAN_POINT('Ctrl Pts',(89.755930604391,-3.72148643608346,0.000620124237849362));
#9876=CARTESIAN_POINT('Ctrl Pts',(89.7621758663193,-3.72148320024645,-0.11604520301192));
#9877=CARTESIAN_POINT('Ctrl Pts',(89.7682938357506,-3.71606355130549,-0.232631117773188));
#9878=CARTESIAN_POINT('Ctrl Pts',(89.7742966682074,-3.70526701499799,-0.348632458025145));
#9879=CARTESIAN_POINT('Ctrl Pts',(89.7803063561815,-3.69445814853769,-0.464766277269504));
#9880=CARTESIAN_POINT('Ctrl Pts',(89.7862007878316,-3.67825993465173,-0.580314274054517));
#9881=CARTESIAN_POINT('Ctrl Pts',(89.7920199315015,-3.65674536414029,-0.694770939840757));
#9882=CARTESIAN_POINT('Ctrl Pts',(89.7978513367025,-3.63518546022771,-0.809468777531487));
#9883=CARTESIAN_POINT('Ctrl Pts',(89.8036073909849,-3.60828645199377,-0.923070712205742));
#9884=CARTESIAN_POINT('Ctrl Pts',(89.809353237266,-3.57615892948402,-1.03506848814753));
#9885=CARTESIAN_POINT('Ctrl Pts',(89.8151055960043,-3.54399499299757,-1.14719320460903));
#9886=CARTESIAN_POINT('Ctrl Pts',(89.8208481430059,-3.50659021610027,-1.25771004248434));
#9887=CARTESIAN_POINT('Ctrl Pts',(89.8266661761538,-3.46409864915259,-1.36610976445866));
#9888=CARTESIAN_POINT('Ctrl Pts',(89.831946043114,-3.42553753842782,-1.46448254715063));
#9889=CARTESIAN_POINT('Ctrl Pts',(89.8372885959291,-3.38278668155183,-1.56111247008492));
#9890=CARTESIAN_POINT('Ctrl Pts',(89.8427666109971,-3.33599933114379,-1.65561882580734));
#9891=CARTESIAN_POINT('Ctrl Pts',(89.8433373580716,-3.33112461958535,-1.66546531680476));
#9892=CARTESIAN_POINT('Ctrl Pts',(89.8439095756265,-3.326206091597,-1.67528880256419));
#9893=CARTESIAN_POINT('Ctrl Pts',(89.8444833459717,-3.32124392029627,-1.6850888851092));
#9894=CARTESIAN_POINT('Ctrl Pts',(89.8474441542933,-3.29563779024094,-1.73565993011997));
#9895=CARTESIAN_POINT('Ctrl Pts',(89.8504464360192,-3.26887033107731,-1.78560634631337));
#9896=CARTESIAN_POINT('Ctrl Pts',(89.8535017500722,-3.24097044142362,-1.83487015331027));
#9897=CARTESIAN_POINT('Ctrl Pts',(89.8535044174161,-3.24094608432016,-1.83491316149629));
#9898=CARTESIAN_POINT('Ctrl Pts',(89.8535070848004,-3.24092172635365,-1.83495616916238));
#9899=CARTESIAN_POINT('Ctrl Pts',(89.8535097522252,-3.24089736752414,-1.83499917630854));
#9900=CARTESIAN_POINT('Ctrl Pts',(89.8589137387239,-3.19154835179572,-1.92212817122396));
#9901=CARTESIAN_POINT('Ctrl Pts',(89.8644938487987,-3.13852061015129,-2.00734601212772));
#9902=CARTESIAN_POINT('Ctrl Pts',(89.8701750604681,-3.08201730534746,-2.09034505631457));
#9903=CARTESIAN_POINT('Ctrl Pts',(89.8707320000666,-3.07647818275871,-2.09848160482437));
#9904=CARTESIAN_POINT('Ctrl Pts',(89.8712899112757,-3.07090569774484,-2.10659681532305));
#9905=CARTESIAN_POINT('Ctrl Pts',(89.8718487234165,-3.06530006698725,-2.11469038882675));
#9906=CARTESIAN_POINT('Ctrl Pts',(89.8780998110759,-3.00259332407221,-2.20522821675504));
#9907=CARTESIAN_POINT('Ctrl Pts',(89.8844631004165,-2.93573350537016,-2.29306097761275));
#9908=CARTESIAN_POINT('Ctrl Pts',(89.8908510398042,-2.86502180238879,-2.37781936750945));
#9909=CARTESIAN_POINT('Ctrl Pts',(89.8972325996347,-2.79438071832383,-2.46249311023463));
#9910=CARTESIAN_POINT('Ctrl Pts',(89.9036384191999,-2.71989569341618,-2.54409887403038));
#9911=CARTESIAN_POINT('Ctrl Pts',(89.909999111458,-2.64189179399096,-2.6223018081862));
#9912=CARTESIAN_POINT('Ctrl Pts',(89.9164074630992,-2.56330342709214,-2.70109070114267));
#9913=CARTESIAN_POINT('Ctrl Pts',(89.9227697801519,-2.48114335343996,-2.7764256997981));
#9914=CARTESIAN_POINT('Ctrl Pts',(89.9290375863566,-2.39576662525555,-2.84799545090647));
#9915=CARTESIAN_POINT('Ctrl Pts',(89.9352525739387,-2.31110936430494,-2.91896208577991));
#9916=CARTESIAN_POINT('Ctrl Pts',(89.9413745830721,-2.22328951831127,-2.98622675999417));
#9917=CARTESIAN_POINT('Ctrl Pts',(89.9473803537221,-2.13267399349501,-3.04951465433723));
#9918=CARTESIAN_POINT('Ctrl Pts',(89.9533856409564,-2.04206576249122,-3.11279745451974));
#9919=CARTESIAN_POINT('Ctrl Pts',(89.9592747054459,-1.94866232073446,-3.1721040811871));
#9920=CARTESIAN_POINT('Ctrl Pts',(89.9650488471482,-1.85285062128836,-3.22718824679365));
#9921=CARTESIAN_POINT('Ctrl Pts',(89.9708240154301,-1.75702188756238,-3.28228220576677));
#9922=CARTESIAN_POINT('Ctrl Pts',(89.9764842926361,-1.65878403119107,-3.33315208754173));
#9923=CARTESIAN_POINT('Ctrl Pts',(89.9820550254397,-1.55854429019367,-3.3795810664276));
#9924=CARTESIAN_POINT('Ctrl Pts',(89.9877080358082,-1.4568240470652,-3.42669578334012));
#9925=CARTESIAN_POINT('Ctrl Pts',(89.9932689499082,-1.3530422664884,-3.46923715542868));
#9926=CARTESIAN_POINT('Ctrl Pts',(89.998787728209,-1.24764593410952,-3.50701223733093));
#9927=CARTESIAN_POINT('Ctrl Pts',(90.0042355328496,-1.14360504002895,-3.54430151681884));
#9928=CARTESIAN_POINT('Ctrl Pts',(90.0096426030432,-1.03799086801436,-3.57694607131596));
#9929=CARTESIAN_POINT('Ctrl Pts',(90.015076291169,-0.93125450523574,-3.60479654993437));
#9930=CARTESIAN_POINT('Ctrl Pts',(90.0206161639213,-0.822432310411888,-3.63319128000809));
#9931=CARTESIAN_POINT('Ctrl Pts',(90.0261841147079,-0.712443581167876,-3.65660210740134));
#9932=CARTESIAN_POINT('Ctrl Pts',(90.0318663644519,-0.601789039154095,-3.67491544567526));
#9933=CARTESIAN_POINT('Ctrl Pts',(90.03687762912,-0.504201072810251,-3.6910662643095));
#9934=CARTESIAN_POINT('Ctrl Pts',(90.0419783102061,-0.406094477094452,-3.70325271084103));
#9935=CARTESIAN_POINT('Ctrl Pts',(90.047232028394,-0.307830069065341,-3.71143138244006));
#9936=CARTESIAN_POINT('Ctrl Pts',(90.0479331053229,-0.294717277907041,-3.71252277671782));
#9937=CARTESIAN_POINT('Ctrl Pts',(90.0486369074277,-0.281601620847862,-3.71354285516211));
#9938=CARTESIAN_POINT('Ctrl Pts',(90.0493435858886,-0.268483902733631,-3.71449156145726));
#9939=CARTESIAN_POINT('Ctrl Pts',(90.0493459763846,-0.268439529153975,-3.71449477066591));
#9940=CARTESIAN_POINT('Ctrl Pts',(90.0493483669136,-0.268395155550725,-3.71449797905786));
#9941=CARTESIAN_POINT('Ctrl Pts',(90.0493507574754,-0.268350781923909,-3.71450118663316));
#9942=CARTESIAN_POINT('Ctrl Pts',(90.0547735338317,-0.167693167150674,-3.72177728510962));
#9943=CARTESIAN_POINT('Ctrl Pts',(90.0603779902922,-0.0666090155227414,
-3.72486349689355));
#9944=CARTESIAN_POINT('Ctrl Pts',(90.0660918238188,0.0345328598509972,-3.72376215121569));
#9945=CARTESIAN_POINT('Ctrl Pts',(90.0667434557154,0.0460675452353268,-3.72363654868116));
#9946=CARTESIAN_POINT('Ctrl Pts',(90.0673965101889,0.0576029372165674,-3.72345651607179));
#9947=CARTESIAN_POINT('Ctrl Pts',(90.0680508799934,0.0691384552651014,-3.72322208374306));
#9948=CARTESIAN_POINT('Ctrl Pts',(90.0744342902308,0.181668011938435,-3.72093518462754));
#9949=CARTESIAN_POINT('Ctrl Pts',(90.0809422787749,0.294214737682507,-3.71346809242457));
#9950=CARTESIAN_POINT('Ctrl Pts',(90.0874852453869,0.406283979113922,-3.70087372346122));
#9951=CARTESIAN_POINT('Ctrl Pts',(90.0940208175582,0.518226567084839,-3.68829358784496));
#9952=CARTESIAN_POINT('Ctrl Pts',(90.1005909100288,0.62969285326157,-3.67059815377306));
#9953=CARTESIAN_POINT('Ctrl Pts',(90.1071233811401,0.740205377944357,-3.64787972663019));
#9954=CARTESIAN_POINT('Ctrl Pts',(90.1136494875706,0.850610228680375,-3.62518343437855));
#9955=CARTESIAN_POINT('Ctrl Pts',(90.1201378312342,0.960063280525032,-3.59747414462497));
#9956=CARTESIAN_POINT('Ctrl Pts',(90.1265380103702,1.0681023280649,-3.56487890111766));
#9957=CARTESIAN_POINT('Ctrl Pts',(90.1329346811574,1.17608215247311,-3.53230152515401));
#9958=CARTESIAN_POINT('Ctrl Pts',(90.1392431880217,1.28264957901568,-3.49484362828946));
#9959=CARTESIAN_POINT('Ctrl Pts',(90.1454370227585,1.38735577890121,-3.45266490700772));
#9960=CARTESIAN_POINT('Ctrl Pts',(90.1516288453074,1.49202796293576,-3.41049988830616));
#9961=CARTESIAN_POINT('Ctrl Pts',(90.1577060655008,1.59484012483382,-3.36361709399763));
#9962=CARTESIAN_POINT('Ctrl Pts',(90.1636667415201,1.69535609174828,-3.3122084954954));
#9963=CARTESIAN_POINT('Ctrl Pts',(90.1696268118186,1.79586184428049,-3.26080512110922));
#9964=CARTESIAN_POINT('Ctrl Pts',(90.1754704396039,1.89407179941306,-3.20487676734605));
#9965=CARTESIAN_POINT('Ctrl Pts',(90.1812196762402,1.98956268415211,-3.14464863508211));
#9966=CARTESIAN_POINT('Ctrl Pts',(90.1869720891323,2.08510632432536,-3.08438722884361));
#9967=CARTESIAN_POINT('Ctrl Pts',(90.1926301759772,2.17792774267623,-3.01982112287708));
#9968=CARTESIAN_POINT('Ctrl Pts',(90.1982382110071,2.26761734407342,-2.95121120649005));
#9969=CARTESIAN_POINT('Ctrl Pts',(90.2038477200996,2.35733052023075,-2.88258325610245));
#9970=CARTESIAN_POINT('Ctrl Pts',(90.2094074409087,2.44390998109456,-2.80990913967479));
#9971=CARTESIAN_POINT('Ctrl Pts',(90.2149804568369,2.52696313645904,-2.73348827855506));
#9972=CARTESIAN_POINT('Ctrl Pts',(90.2205596467886,2.610108301635,-2.65698275516099));
#9973=CARTESIAN_POINT('Ctrl Pts',(90.2261526023147,2.68971893078859,-2.57672191582007));
#9974=CARTESIAN_POINT('Ctrl Pts',(90.2318359798101,2.76542342787462,-2.49304835781216));
#9975=CARTESIAN_POINT('Ctrl Pts',(90.2364352263609,2.82668693665691,-2.42533592389905));
#9976=CARTESIAN_POINT('Ctrl Pts',(90.24109409516,2.88539266671139,-2.35538933141771));
#9977=CARTESIAN_POINT('Ctrl Pts',(90.2458560731707,2.94135779478508,-2.28341200968227));
#9978=CARTESIAN_POINT('Ctrl Pts',(90.2458574776968,2.94137430147326,-2.28339078026233));
#9979=CARTESIAN_POINT('Ctrl Pts',(90.2458588822319,2.94139080792326,-2.28336955066568));
#9980=CARTESIAN_POINT('Ctrl Pts',(90.245860286776,2.94140731413508,-2.28334832089232));
#9981=CARTESIAN_POINT('Ctrl Pts',(90.2517448434871,3.01056266485227,-2.19440287183321));
#9982=CARTESIAN_POINT('Ctrl Pts',(90.2577943942158,3.07566668485485,-2.10217505882779));
#9983=CARTESIAN_POINT('Ctrl Pts',(90.2639263439004,3.13644516681204,-2.00709297216542));
#9984=CARTESIAN_POINT('Ctrl Pts',(90.2700534151133,3.19717529447501,-1.91208653114349));
#9985=CARTESIAN_POINT('Ctrl Pts',(90.2762623875696,3.25358714427209,-1.81423050772147));
#9986=CARTESIAN_POINT('Ctrl Pts',(90.2824903460121,3.30544864642787,-1.71396457622133));
#9987=CARTESIAN_POINT('Ctrl Pts',(90.2887148681921,3.3572815341123,-1.61375396623144));
#9988=CARTESIAN_POINT('Ctrl Pts',(90.2949581587654,3.40456932356956,-1.51113613082438));
#9989=CARTESIAN_POINT('Ctrl Pts',(90.3011810498467,3.44711720445529,-1.40656138592201));
#9990=CARTESIAN_POINT('Ctrl Pts',(90.3074019107302,3.48965120423418,-1.30202075818778));
#9991=CARTESIAN_POINT('Ctrl Pts',(90.3136023159836,3.52744847020503,-1.19552446407259));
#9992=CARTESIAN_POINT('Ctrl Pts',(90.3197687339331,3.56034892071842,-1.08753386357061));
#9993=CARTESIAN_POINT('Ctrl Pts',(90.3259354487432,3.5932509551087,-0.979538064239594));
#9994=CARTESIAN_POINT('Ctrl Pts',(90.3320682076598,3.62125565042711,-0.870047759469028));
#9995=CARTESIAN_POINT('Ctrl Pts',(90.3381793344755,3.64423723377603,-0.759536554368533));
#9996=CARTESIAN_POINT('Ctrl Pts',(90.3406749151909,3.65362214722101,-0.714407457786194));
#9997=CARTESIAN_POINT('Ctrl Pts',(90.3431671843077,3.66216979237232,-0.669108258246237));
#9998=CARTESIAN_POINT('Ctrl Pts',(90.345658177608,3.66987330948582,-0.62367182598591));
#9999=CARTESIAN_POINT('Ctrl Pts',(90.3456586167391,3.66987466751999,-0.623663816108521));
#10000=CARTESIAN_POINT('Ctrl Pts',(90.3456590558701,3.66987602552788,-0.623655806227113));
#10001=CARTESIAN_POINT('Ctrl Pts',(90.3456594950011,3.66987738350949,-0.623647796341697));
#10002=CARTESIAN_POINT('Ctrl Pts',(90.3524840062436,3.69098170271146,-0.499166597645409));
#10003=CARTESIAN_POINT('Ctrl Pts',(90.3592950968009,3.70573899079509,-0.373714783119458));
#10004=CARTESIAN_POINT('Ctrl Pts',(90.3660689121749,3.71411672006159,-0.247903770232333));
#10005=CARTESIAN_POINT('Ctrl Pts',(90.3728585237779,3.7225139858113,-0.12179937179144));
#10006=CARTESIAN_POINT('Ctrl Pts',(90.3796106154978,3.72450199002899,0.00466615234247741));
#10007=CARTESIAN_POINT('Ctrl Pts',(90.3863244864897,3.72008560322385,0.130880164094778));
#10008=CARTESIAN_POINT('Ctrl Pts',(90.393041252459,3.71566731210153,0.257148598505923));
#10009=CARTESIAN_POINT('Ctrl Pts',(90.3997198692073,3.70483896923014,0.383165532035909));
#10010=CARTESIAN_POINT('Ctrl Pts',(90.4063826830949,3.68764344224471,0.5083169351252));
#10011=CARTESIAN_POINT('Ctrl Pts',(90.4130415494875,3.67045810303578,0.633394190180367));
#10012=CARTESIAN_POINT('Ctrl Pts',(90.419684914363,3.64691277564379,0.757607069371454));
#10013=CARTESIAN_POINT('Ctrl Pts',(90.4263552072003,3.61709182197542,0.880339277295861));
#10014=CARTESIAN_POINT('Ctrl Pts',(90.4318741295373,3.59241831343142,0.981886471745885));
#10015=CARTESIAN_POINT('Ctrl Pts',(90.4374119961341,3.56344927633743,1.082419944246));
#10016=CARTESIAN_POINT('Ctrl Pts',(90.4430005297901,3.53025723298489,1.18158852036477));
#10017=CARTESIAN_POINT('Ctrl Pts',(89.7566589985681,-3.72274994162807,0.00065924818494276));
#10018=CARTESIAN_POINT('Ctrl Pts',(89.754692356951,-3.72274344729714,0.0373324930346883));
#10019=CARTESIAN_POINT('Ctrl Pts',(89.7527097850186,-3.72219504574113,0.0740027969240078));
#10020=CARTESIAN_POINT('Ctrl Pts',(89.7481085869829,-3.71968528510386,0.158398523147372));
#10021=CARTESIAN_POINT('Ctrl Pts',(89.7454793224464,-3.71734703073846,0.206105536755127));
#10022=CARTESIAN_POINT('Ctrl Pts',(89.7275651638507,-3.69537905180333,0.527642985931046));
#10023=CARTESIAN_POINT('Ctrl Pts',(89.7114316014278,-3.64642915685228,0.798592725572422));
#10024=CARTESIAN_POINT('Ctrl Pts',(89.6889378155214,-3.53714918903783,1.16587590463302));
#10025=CARTESIAN_POINT('Ctrl Pts',(89.6825811181009,-3.50158739501498,1.26869164843413));
#10026=CARTESIAN_POINT('Ctrl Pts',(89.6723642039251,-3.43597870109353,1.43448835134085));
#10027=CARTESIAN_POINT('Ctrl Pts',(89.6684320771745,-3.40857351286186,1.49844390509589));
#10028=CARTESIAN_POINT('Ctrl Pts',(89.6628287522555,-3.36608403513711,1.59039370623631));
#10029=CARTESIAN_POINT('Ctrl Pts',(89.6610915574921,-3.35240934010757,1.6190199570756));
#10030=CARTESIAN_POINT('Ctrl Pts',(89.6579877322658,-3.32702422154747,1.67045942330549));
#10031=CARTESIAN_POINT('Ctrl Pts',(89.6566145446623,-3.31544171565319,1.69333137616355));
#10032=CARTESIAN_POINT('Ctrl Pts',(89.6533322295204,-3.28690625779162,1.74826481963309));
#10033=CARTESIAN_POINT('Ctrl Pts',(89.6514364501536,-3.26971971795486,1.78020105101389));
#10034=CARTESIAN_POINT('Ctrl Pts',(89.6443192861104,-3.20264969025658,1.90058213208958));
#10035=CARTESIAN_POINT('Ctrl Pts',(89.6392559566166,-3.14961899067667,1.9872293465319));
#10036=CARTESIAN_POINT('Ctrl Pts',(89.6224653878367,-2.95888814319197,2.27200911067671));
#10037=CARTESIAN_POINT('Ctrl Pts',(89.6111551859286,-2.80550814796508,2.45889715906491));
#10038=CARTESIAN_POINT('Ctrl Pts',(89.5990569744384,-2.63046736566053,2.63430302642997));
#10039=CARTESIAN_POINT('Ctrl Pts',(89.5987349289147,-2.62579979151321,2.63895555994337));
#10040=CARTESIAN_POINT('Ctrl Pts',(89.5984125828093,-2.62112000663417,2.64359555781933));
#10041=CARTESIAN_POINT('Origin',(81.4430005297901,0.,0.));
#10042=CARTESIAN_POINT('',(82.8483099710866,-4.43364346784955,0.00310368774765633));
#10043=CARTESIAN_POINT('',(82.4452259247167,1.97302819977468,3.97206321802814));
#10044=CARTESIAN_POINT('Ctrl Pts',(82.8483099710627,-4.43364346785048,0.00310368833033136));
#10045=CARTESIAN_POINT('Ctrl Pts',(82.8431982004951,-4.4338383207308,0.127632029051098));
#10046=CARTESIAN_POINT('Ctrl Pts',(82.8380437813906,-4.42875792909011,0.252000944091934));
#10047=CARTESIAN_POINT('Ctrl Pts',(82.8327597771156,-4.4184097134055,0.375824375914131));
#10048=CARTESIAN_POINT('Ctrl Pts',(82.8297019360816,-4.41242122495965,0.447480709082303));
#10049=CARTESIAN_POINT('Ctrl Pts',(82.8266006981391,-4.40466844329161,0.518955322921443));
#10050=CARTESIAN_POINT('Ctrl Pts',(82.8234392149119,-4.39515054133119,0.590181060107312));
#10051=CARTESIAN_POINT('Ctrl Pts',(82.8216860236884,-4.38987241679758,0.629679083141025));
#10052=CARTESIAN_POINT('Ctrl Pts',(82.8199141716151,-4.38405193541917,0.669099352470447));
#10053=CARTESIAN_POINT('Ctrl Pts',(82.8181206431555,-4.3776895649354,0.70842910067796));
#10054=CARTESIAN_POINT('Ctrl Pts',(82.8181187212864,-4.3776827472888,0.708471244769515));
#10055=CARTESIAN_POINT('Ctrl Pts',(82.8181167993924,-4.37767592901998,0.708513388757189));
#10056=CARTESIAN_POINT('Ctrl Pts',(82.8181148774735,-4.37766911012896,0.708555532640965));
#10057=CARTESIAN_POINT('Ctrl Pts',(82.8129148389423,-4.3592195821887,0.822582103675738));
#10058=CARTESIAN_POINT('Ctrl Pts',(82.8075272992602,-4.33618224457112,0.93601237641731));
#10059=CARTESIAN_POINT('Ctrl Pts',(82.8020295457792,-4.30864871846121,1.04846335123121));
#10060=CARTESIAN_POINT('Ctrl Pts',(82.8014868661422,-4.3059309021735,1.05956331313577));
#10061=CARTESIAN_POINT('Ctrl Pts',(82.8009431126332,-4.30316930831883,1.07065370525351));
#10062=CARTESIAN_POINT('Ctrl Pts',(82.8003983595855,-4.30036404582785,1.08173414129563));
#10063=CARTESIAN_POINT('Ctrl Pts',(82.7943421099015,-4.26917675803463,1.20492002811735));
#10064=CARTESIAN_POINT('Ctrl Pts',(82.7881628508326,-4.23258800048932,1.32687961667018));
#10065=CARTESIAN_POINT('Ctrl Pts',(82.7819515177903,-4.19076317124117,1.44713010522075));
#10066=CARTESIAN_POINT('Ctrl Pts',(82.775746103116,-4.14897819410393,1.5672660150416));
#10067=CARTESIAN_POINT('Ctrl Pts',(82.7695090211858,-4.10196745579517,1.68569623676777));
#10068=CARTESIAN_POINT('Ctrl Pts',(82.763313229815,-4.04993106810721,1.80196281954222));
#10069=CARTESIAN_POINT('Ctrl Pts',(82.7581865020976,-4.00687338990092,1.898167981539));
#10070=CARTESIAN_POINT('Ctrl Pts',(82.7530883257333,-3.96037342239628,1.99289395940686));
#10071=CARTESIAN_POINT('Ctrl Pts',(82.7481264079222,-3.91044593450664,2.0858223196227));
#10072=CARTESIAN_POINT('Ctrl Pts',(82.7467858018045,-3.89695657449428,2.11092961340606));
#10073=CARTESIAN_POINT('Ctrl Pts',(82.7454551421122,-3.88321715603325,2.13590542803796));
#10074=CARTESIAN_POINT('Ctrl Pts',(82.7441365530662,-3.86922830218736,2.16074292003209));
#10075=CARTESIAN_POINT('Ctrl Pts',(82.7393269478812,-3.81820340994339,2.25133864478362));
#10076=CARTESIAN_POINT('Ctrl Pts',(82.7346478456743,-3.76390741767749,2.34011631238078));
#10077=CARTESIAN_POINT('Ctrl Pts',(82.7299933208539,-3.70666292796658,2.42695743283104));
#10078=CARTESIAN_POINT('Ctrl Pts',(82.7289460935899,-3.69378341982112,2.44649592332766));
#10079=CARTESIAN_POINT('Ctrl Pts',(82.7279001104591,-3.68075453556109,2.46593655474058));
#10080=CARTESIAN_POINT('Ctrl Pts',(82.7268541650439,-3.66757973118956,2.4852782682022));
#10081=CARTESIAN_POINT('Ctrl Pts',(82.7211602299211,-3.595858511079,2.59057101102986));
#10082=CARTESIAN_POINT('Ctrl Pts',(82.7154673659965,-3.51981327232184,2.69293423205903));
#10083=CARTESIAN_POINT('Ctrl Pts',(82.7097732753536,-3.43970668251573,2.79202036852321));
#10084=CARTESIAN_POINT('Ctrl Pts',(82.7045389955647,-3.3660688832119,2.88310507264559));
#10085=CARTESIAN_POINT('Ctrl Pts',(82.6993036398664,-3.28899541526,2.9714242342106));
#10086=CARTESIAN_POINT('Ctrl Pts',(82.6941566462714,-3.20857965293882,3.05657768639395));
#10087=CARTESIAN_POINT('Ctrl Pts',(82.6937040853997,-3.20150891799011,3.06406499327231));
#10088=CARTESIAN_POINT('Ctrl Pts',(82.6932522076729,-3.1944123615882,3.07152779766707));
#10089=CARTESIAN_POINT('Ctrl Pts',(82.6928010738893,-3.18729005828529,3.07896581173227));
#10090=CARTESIAN_POINT('Ctrl Pts',(82.6885158565976,-3.11963691772868,3.14961781707563));
#10091=CARTESIAN_POINT('Ctrl Pts',(82.6844125514995,-3.04952028554853,3.2178922091441));
#10092=CARTESIAN_POINT('Ctrl Pts',(82.6803745937489,-2.9772327649036,3.28372831794796));
#10093=CARTESIAN_POINT('Ctrl Pts',(82.6791511744965,-2.95533111314611,3.30367532284211));
#10094=CARTESIAN_POINT('Ctrl Pts',(82.6779337539151,-2.9332299348907,3.3233987677457));
#10095=CARTESIAN_POINT('Ctrl Pts',(82.6767190900405,-2.9109367004746,3.34289763278784));
#10096=CARTESIAN_POINT('Ctrl Pts',(82.6714898824389,-2.8149628649872,3.42684152494881));
#10097=CARTESIAN_POINT('Ctrl Pts',(82.6663115200674,-2.71543044857947,3.50662209046862));
#10098=CARTESIAN_POINT('Ctrl Pts',(82.6611172833366,-2.61272339386486,3.58191009741878));
#10099=CARTESIAN_POINT('Ctrl Pts',(82.6559198850698,-2.50995382523878,3.65724392933993));
#10100=CARTESIAN_POINT('Ctrl Pts',(82.6507062078556,-2.40400557751432,3.72807934776612));
#10101=CARTESIAN_POINT('Ctrl Pts',(82.6453940202299,-2.29529843068837,3.7941160661364));
#10102=CARTESIAN_POINT('Ctrl Pts',(82.6405334395281,-2.19583284376807,3.85453878113515));
#10103=CARTESIAN_POINT('Ctrl Pts',(82.6355899255016,-2.09405699856372,3.91094430538531));
#10104=CARTESIAN_POINT('Ctrl Pts',(82.6304940642063,-1.99032227923783,3.96312847935643));
#10105=CARTESIAN_POINT('Ctrl Pts',(82.6300128876823,-1.98052713200542,3.96805596815257));
#10106=CARTESIAN_POINT('Ctrl Pts',(82.6295303528188,-1.97071450152822,3.97294585314192));
#10107=CARTESIAN_POINT('Ctrl Pts',(82.6290464011762,-1.9608846720785,3.97779798356357));
#10108=CARTESIAN_POINT('Ctrl Pts',(82.6270433239479,-1.92019897996788,3.99788096520893));
#10109=CARTESIAN_POINT('Ctrl Pts',(82.625015938978,-1.87921937340591,4.01731684720352));
#10110=CARTESIAN_POINT('Ctrl Pts',(82.6229600729164,-1.83796794857875,4.03609494548256));
#10111=CARTESIAN_POINT('Ctrl Pts',(82.6229578270958,-1.83792288567218,4.03611545860888));
#10112=CARTESIAN_POINT('Ctrl Pts',(82.6229555812412,-1.83787782244118,4.03613597095037));
#10113=CARTESIAN_POINT('Ctrl Pts',(82.6229533353526,-1.8378327588858,4.03615648250706));
#10114=CARTESIAN_POINT('Ctrl Pts',(82.6178327674325,-1.73508901790095,4.08292230135918));
#10115=CARTESIAN_POINT('Ctrl Pts',(82.6125243072668,-1.63034728655921,4.12573969567118));
#10116=CARTESIAN_POINT('Ctrl Pts',(82.6071032863895,-1.5239600949963,4.16447005790881));
#10117=CARTESIAN_POINT('Ctrl Pts',(82.6065744137859,-1.51358100362888,4.16824857637942));
#10118=CARTESIAN_POINT('Ctrl Pts',(82.6060444698436,-1.50318629019696,4.17198820670683));
#10119=CARTESIAN_POINT('Ctrl Pts',(82.6055135245124,-1.4927763072773,4.17568882823057));
#10120=CARTESIAN_POINT('Ctrl Pts',(82.5995477274928,-1.37580787112226,4.21726967574725));
#10121=CARTESIAN_POINT('Ctrl Pts',(82.5934560145702,-1.25690592807626,4.25392421717051));
#10122=CARTESIAN_POINT('Ctrl Pts',(82.5873277913627,-1.1365420839014,4.28551969062002));
#10123=CARTESIAN_POINT('Ctrl Pts',(82.5812054988219,-1.0162947233816,4.31708458714458));
#10124=CARTESIAN_POINT('Ctrl Pts',(82.5750471072853,-0.89458839386563,4.34360053668037));
#10125=CARTESIAN_POINT('Ctrl Pts',(82.5689255999665,-0.77189485234871,4.36497801511059));
#10126=CARTESIAN_POINT('Ctrl Pts',(82.5644289908867,-0.681769191447175,
4.38068103703099));
#10127=CARTESIAN_POINT('Ctrl Pts',(82.5599523947277,-0.591107837079897,
4.39361192698146));
#10128=CARTESIAN_POINT('Ctrl Pts',(82.5556188258972,-0.500087401159369,
4.40357392969721));
#10129=CARTESIAN_POINT('Ctrl Pts',(82.5540567867667,-0.467278995859554,
4.40716474333583));
#10130=CARTESIAN_POINT('Ctrl Pts',(82.5525133304488,-0.434424426428198,
4.41036978328745));
#10131=CARTESIAN_POINT('Ctrl Pts',(82.5509942179002,-0.401533624456914,
4.41317976781749));
#10132=CARTESIAN_POINT('Ctrl Pts',(82.5460952165885,-0.295463746915021,
4.42224171514418));
#10133=CARTESIAN_POINT('Ctrl Pts',(82.5413174954551,-0.189042120070781,
4.42742225121933));
#10134=CARTESIAN_POINT('Ctrl Pts',(82.536558687016,-0.0825715696876148,
4.42892500778567));
#10135=CARTESIAN_POINT('Ctrl Pts',(82.5357498825313,-0.0644758930611303,
4.4291804154714));
#10136=CARTESIAN_POINT('Ctrl Pts',(82.5349416243627,-0.0463786813114588,
4.42932958564746));
#10137=CARTESIAN_POINT('Ctrl Pts',(82.5341334099387,-0.0282812715984249,
4.42937351348461));
#10138=CARTESIAN_POINT('Ctrl Pts',(82.5262973875791,0.14718170324818,4.42979941471063));
#10139=CARTESIAN_POINT('Ctrl Pts',(82.5184653978724,0.322665269126018,4.42033670888078));
#10140=CARTESIAN_POINT('Ctrl Pts',(82.5106321803695,0.497009262517875,4.40107786738388));
#10141=CARTESIAN_POINT('Ctrl Pts',(82.5073424783614,0.570228190110464,4.39298976699313));
#10142=CARTESIAN_POINT('Ctrl Pts',(82.5040525680356,0.643245945700422,4.38317325741542));
#10143=CARTESIAN_POINT('Ctrl Pts',(82.5007620893839,0.715975650346953,4.37163257845778));
#10144=CARTESIAN_POINT('Ctrl Pts',(82.4967352603142,0.80498096534671,4.35750930144286));
#10145=CARTESIAN_POINT('Ctrl Pts',(82.4927075574528,0.893559613112715,4.34080280069945));
#10146=CARTESIAN_POINT('Ctrl Pts',(82.4888009173514,0.981485590988129,4.32131589256869));
#10147=CARTESIAN_POINT('Ctrl Pts',(82.4873052817133,1.01514756716311,4.31385543715981));
#10148=CARTESIAN_POINT('Ctrl Pts',(82.4858273902324,1.04871334781174,4.30598756179976));
#10149=CARTESIAN_POINT('Ctrl Pts',(82.4843740851927,1.08216828460725,4.29770167811292));
#10150=CARTESIAN_POINT('Ctrl Pts',(82.480001238261,1.18283078402603,4.2727702975245));
#10151=CARTESIAN_POINT('Ctrl Pts',(82.4757657178508,1.28252133410666,4.24419825053364));
#10152=CARTESIAN_POINT('Ctrl Pts',(82.4715597827366,1.38098904233782,4.21219023683576));
#10153=CARTESIAN_POINT('Ctrl Pts',(82.47071405811,1.40078881658986,4.20575410201695));
#10154=CARTESIAN_POINT('Ctrl Pts',(82.4698695296969,1.42053931409565,4.1991790123273));
#10155=CARTESIAN_POINT('Ctrl Pts',(82.4690253215438,1.44023874403481,4.19246657992103));
#10156=CARTESIAN_POINT('Ctrl Pts',(82.4639755178385,1.5580749126782,4.15231479281467));
#10157=CARTESIAN_POINT('Ctrl Pts',(82.4589368589213,1.67408104493834,4.10724876386509));
#10158=CARTESIAN_POINT('Ctrl Pts',(82.4538338262441,1.7878010490968,4.05744660917939));
#10159=CARTESIAN_POINT('Ctrl Pts',(82.4510432927973,1.84998749689243,4.03021288618236));
#10160=CARTESIAN_POINT('Ctrl Pts',(82.4482332511581,1.91149046456204,4.00156368429464));
#10161=CARTESIAN_POINT('Ctrl Pts',(82.4453899175418,1.97223673451587,3.97153404972695));
#10162=CARTESIAN_POINT('',(82.4430005297901,-1.97158113240048,3.97043534620102));
#10163=CARTESIAN_POINT('Origin',(82.4430005297901,0.,0.));
#10164=CARTESIAN_POINT('',(82.6635449442269,-4.43315179037873,0.0011479234960335));
#10165=CARTESIAN_POINT('Ctrl Pts',(82.4430005297901,-1.97158113240048,3.97043534620102));
#10166=CARTESIAN_POINT('Ctrl Pts',(82.4459140470573,-2.02972790039701,3.94156166845641));
#10167=CARTESIAN_POINT('Ctrl Pts',(82.4488510668016,-2.08723260366219,3.91141452221414));
#10168=CARTESIAN_POINT('Ctrl Pts',(82.4577025121475,-2.2575544382045,3.8172965693948));
#10169=CARTESIAN_POINT('Ctrl Pts',(82.4636592841556,-2.36824732103486,3.74962785239478));
#10170=CARTESIAN_POINT('Ctrl Pts',(82.4782616257372,-2.63154904369224,3.57235033341775));
#10171=CARTESIAN_POINT('Ctrl Pts',(82.4868979764478,-2.78046866885149,3.45770631344884));
#10172=CARTESIAN_POINT('Ctrl Pts',(82.5030578932604,-3.0472355141486,3.22392913955234));
#10173=CARTESIAN_POINT('Ctrl Pts',(82.5105870370778,-3.16648552289963,3.10688511384025));
#10174=CARTESIAN_POINT('Ctrl Pts',(82.5301318685963,-3.46110369168554,2.78308949972469));
#10175=CARTESIAN_POINT('Ctrl Pts',(82.5420223880646,-3.62462358748545,2.56650253995901));
#10176=CARTESIAN_POINT('Ctrl Pts',(82.5650048709782,-3.90251929498455,2.11839683055745));
#10177=CARTESIAN_POINT('Ctrl Pts',(82.5759565558287,-4.01851747108689,1.88912280783753));
#10178=CARTESIAN_POINT('Ctrl Pts',(82.5973131753662,-4.20610848430369,1.42170340030805));
#10179=CARTESIAN_POINT('Ctrl Pts',(82.6076937618501,-4.2788215920027,1.18501630825411));
#10180=CARTESIAN_POINT('Ctrl Pts',(82.6208977765467,-4.34285070554643,0.891076505103667));
#10181=CARTESIAN_POINT('Ctrl Pts',(82.623275823123,-4.35332048581509,0.838433112605661));
#10182=CARTESIAN_POINT('Ctrl Pts',(82.6275113760015,-4.37004809604923,0.745537923488229));
#10183=CARTESIAN_POINT('Ctrl Pts',(82.6293558561636,-4.37671187288937,0.705365293883261));
#10184=CARTESIAN_POINT('Ctrl Pts',(82.6328942474834,-4.3883004437183,0.629000742213165));
#10185=CARTESIAN_POINT('Ctrl Pts',(82.6345839545017,-4.39333327460925,0.592828279565368));
#10186=CARTESIAN_POINT('Ctrl Pts',(82.6392248750366,-4.40578396093067,0.494450154625385));
#10187=CARTESIAN_POINT('Ctrl Pts',(82.6422126649266,-4.41233088898492,0.432144434949856));
#10188=CARTESIAN_POINT('Ctrl Pts',(82.6511917295901,-4.42781583262629,0.247126109229468));
#10189=CARTESIAN_POINT('Ctrl Pts',(82.6572970613572,-4.43296811398252,0.124159609381366));
#10190=CARTESIAN_POINT('Ctrl Pts',(82.6634574424051,-4.43299985245739,0.00114372756053367));
#10191=CARTESIAN_POINT('',(83.915600810406,-4.42944218562652,-0.000347422039578779));
#10192=CARTESIAN_POINT('Ctrl Pts',(82.6635449442269,-4.43315179037873,0.00114792349603368));
#10193=CARTESIAN_POINT('Ctrl Pts',(82.6697535422384,-4.43290168749669,-0.126097675849478));
#10194=CARTESIAN_POINT('Ctrl Pts',(82.6760083411183,-4.42714199085535,-0.253438677504856));
#10195=CARTESIAN_POINT('Ctrl Pts',(82.6822350885931,-4.4159129991645,-0.380374531670116));
#10196=CARTESIAN_POINT('Ctrl Pts',(82.6862669568839,-4.40864213813809,-0.462566502268552));
#10197=CARTESIAN_POINT('Ctrl Pts',(82.6900873253285,-4.39873439968036,-0.544553531573465));
#10198=CARTESIAN_POINT('Ctrl Pts',(82.6938299895795,-4.38647203791183,-0.626197505433351));
#10199=CARTESIAN_POINT('Ctrl Pts',(82.6958632937083,-4.37981017643023,-0.670552814380214));
#10200=CARTESIAN_POINT('Ctrl Pts',(82.697873663436,-4.37245333657578,-0.71480777713799));
#10201=CARTESIAN_POINT('Ctrl Pts',(82.699882552671,-4.36444623982428,-0.758946675668096));
#10202=CARTESIAN_POINT('Ctrl Pts',(82.7072473607457,-4.3350913456947,-0.920764714535287));
#10203=CARTESIAN_POINT('Ctrl Pts',(82.7146085283909,-4.29702613331697,-1.08103278384968));
#10204=CARTESIAN_POINT('Ctrl Pts',(82.7219689832407,-4.25060656947618,-1.2388514253652));
#10205=CARTESIAN_POINT('Ctrl Pts',(82.7298622375662,-4.20082684382732,-1.40809404694312));
#10206=CARTESIAN_POINT('Ctrl Pts',(82.7377548970905,-4.14143940568037,-1.57452592045708));
#10207=CARTESIAN_POINT('Ctrl Pts',(82.7456521057249,-4.07283034190275,-1.7370584266606));
#10208=CARTESIAN_POINT('Ctrl Pts',(82.7475014553387,-4.0567636338451,-1.77511990401166));
#10209=CARTESIAN_POINT('Ctrl Pts',(82.7493510529934,-4.04019102741035,-1.81296741700496));
#10210=CARTESIAN_POINT('Ctrl Pts',(82.7512009627978,-4.0231171363229,-1.85058674534914));
#10211=CARTESIAN_POINT('Ctrl Pts',(82.7569077384329,-3.97044599234479,-1.96663838521422));
#10212=CARTESIAN_POINT('Ctrl Pts',(82.7626175306464,-3.91300409043966,-2.08052044276572));
#10213=CARTESIAN_POINT('Ctrl Pts',(82.7683204612542,-3.85091206751601,-2.19178529820373));
#10214=CARTESIAN_POINT('Ctrl Pts',(82.7719807173375,-3.81106015272649,-2.26319733036503));
#10215=CARTESIAN_POINT('Ctrl Pts',(82.7754195184539,-3.76896543646566,-2.33334009894391));
#10216=CARTESIAN_POINT('Ctrl Pts',(82.7787739803614,-3.72489414217142,-2.40217518693356));
#10217=CARTESIAN_POINT('Ctrl Pts',(82.7806520316568,-3.70022009499944,-2.4407136559153));
#10218=CARTESIAN_POINT('Ctrl Pts',(82.7825036467726,-3.67492610882491,-2.47884309045198));
#10219=CARTESIAN_POINT('Ctrl Pts',(82.7843528882297,-3.64905554361889,-2.51656304323995));
#10220=CARTESIAN_POINT('Ctrl Pts',(82.7895081501627,-3.57693432900977,-2.62171763837164));
#10221=CARTESIAN_POINT('Ctrl Pts',(82.7946452802066,-3.50033122955016,-2.7236900114497));
#10222=CARTESIAN_POINT('Ctrl Pts',(82.7998383961552,-3.41954196534363,-2.82206378685053));
#10223=CARTESIAN_POINT('Ctrl Pts',(82.804746494571,-3.34318671666422,-2.91503844329819));
#10224=CARTESIAN_POINT('Ctrl Pts',(82.8097050153416,-3.2630918453971,-3.00479882243312));
#10225=CARTESIAN_POINT('Ctrl Pts',(82.8147857671755,-3.17954463462073,-3.09101035441384));
#10226=CARTESIAN_POINT('Ctrl Pts',(82.8150898768471,-3.17454389542689,-3.09617056721964));
#10227=CARTESIAN_POINT('Ctrl Pts',(82.8153944244299,-3.16953078459027,-3.10131808095286));
#10228=CARTESIAN_POINT('Ctrl Pts',(82.8156994253226,-3.16450536241097,-3.10645282965993));
#10229=CARTESIAN_POINT('Ctrl Pts',(82.8207194321271,-3.08179198636384,-3.19096560999218));
#10230=CARTESIAN_POINT('Ctrl Pts',(82.825862755279,-2.99574477245991,-3.27201555267624));
#10231=CARTESIAN_POINT('Ctrl Pts',(82.8312003612335,-2.90667527770515,-3.34930710644914));
#10232=CARTESIAN_POINT('Ctrl Pts',(82.8312023843414,-2.90664151777541,-3.3493364021966));
#10233=CARTESIAN_POINT('Ctrl Pts',(82.8312044074773,-2.90660775741141,-3.34936569740487));
#10234=CARTESIAN_POINT('Ctrl Pts',(82.831206430641,-2.90657399661315,-3.34939499207396));
#10235=CARTESIAN_POINT('Ctrl Pts',(82.8363572762157,-2.82062116310868,-3.42397734631702));
#10236=CARTESIAN_POINT('Ctrl Pts',(82.841700361716,-2.73158702110858,-3.49528321595245));
#10237=CARTESIAN_POINT('Ctrl Pts',(82.8471575515268,-2.63977466411272,-3.56307841028072));
#10238=CARTESIAN_POINT('Ctrl Pts',(82.8477049420542,-2.63056530613615,-3.56987869549384));
#10239=CARTESIAN_POINT('Ctrl Pts',(82.8482534806254,-2.62132803877145,-3.57664365679372));
#10240=CARTESIAN_POINT('Ctrl Pts',(82.8488030883847,-2.61206319676825,-3.58337305721038));
#10241=CARTESIAN_POINT('Ctrl Pts',(82.8548238049242,-2.51057083873772,-3.65709074351118));
#10242=CARTESIAN_POINT('Ctrl Pts',(82.8609723051984,-2.40576350692455,-3.72654164247399));
#10243=CARTESIAN_POINT('Ctrl Pts',(82.8671559578527,-2.29806345963243,-3.79146048281249));
#10244=CARTESIAN_POINT('Ctrl Pts',(82.8733328329235,-2.19048145681947,-3.85630816895108));
#10245=CARTESIAN_POINT('Ctrl Pts',(82.879544443025,-2.08001323879596,-3.91663404207498));
#10246=CARTESIAN_POINT('Ctrl Pts',(82.8857158943829,-1.96709267257739,-3.972213696294));
#10247=CARTESIAN_POINT('Ctrl Pts',(82.8900077147347,-1.88856417804148,-4.01086552668066));
#10248=CARTESIAN_POINT('Ctrl Pts',(82.8942800162594,-1.80884676597104,-4.04722325500299));
#10249=CARTESIAN_POINT('Ctrl Pts',(82.8984045010245,-1.72802482212208,-4.08104405161748));
#10250=CARTESIAN_POINT('Ctrl Pts',(82.9002058966658,-1.69272531062903,-4.09581550528394));
#10251=CARTESIAN_POINT('Ctrl Pts',(82.9019790953342,-1.65721572201682,-4.11010276553236));
#10252=CARTESIAN_POINT('Ctrl Pts',(82.9037134080104,-1.62150602886537,-4.12388455513962));
#10253=CARTESIAN_POINT('Ctrl Pts',(82.9094157471257,-1.50409422483852,-4.1691984359855));
#10254=CARTESIAN_POINT('Ctrl Pts',(82.9150416488362,-1.38474146504016,-4.20960104440071));
#10255=CARTESIAN_POINT('Ctrl Pts',(82.9206660839083,-1.26393293989382,-4.24512429519591));
#10256=CARTESIAN_POINT('Ctrl Pts',(82.9281829542762,-1.10247636492875,-4.29259993814471));
#10257=CARTESIAN_POINT('Ctrl Pts',(82.9356972835923,-0.938412063536249,
-4.33136558777071));
#10258=CARTESIAN_POINT('Ctrl Pts',(82.9432144689425,-0.772724773604452,
-4.36119264732472));
#10259=CARTESIAN_POINT('Ctrl Pts',(82.9469438926373,-0.690524046043502,
-4.37599043898003));
#10260=CARTESIAN_POINT('Ctrl Pts',(82.9506740056613,-0.607923936337747,
-4.38858727479971));
#10261=CARTESIAN_POINT('Ctrl Pts',(82.9544054051174,-0.525045504401398,
-4.39895043695672));
#10262=CARTESIAN_POINT('Ctrl Pts',(82.9581359118733,-0.442186900304788,
-4.40931111983035));
#10263=CARTESIAN_POINT('Ctrl Pts',(82.9618677244815,-0.359045347278706,
-4.41743945724858));
#10264=CARTESIAN_POINT('Ctrl Pts',(82.965469567743,-0.27574647201453,-4.42307138832066));
#10265=CARTESIAN_POINT('Ctrl Pts',(82.9673012120467,-0.233386519262133,
-4.42593539258676));
#10266=CARTESIAN_POINT('Ctrl Pts',(82.9690992459571,-0.19098671178188,-4.42815373228215));
#10267=CARTESIAN_POINT('Ctrl Pts',(82.9708464058618,-0.14856873889832,-4.4296914588579));
#10268=CARTESIAN_POINT('Ctrl Pts',(82.9760346635733,-0.0226069569703721,
-4.4342577963425));
#10269=CARTESIAN_POINT('Ctrl Pts',(82.9811221551682,0.103488754728788,-4.43342346283101));
#10270=CARTESIAN_POINT('Ctrl Pts',(82.9862060321369,0.229218662760157,-4.42723651800783));
#10271=CARTESIAN_POINT('Ctrl Pts',(82.9912928436474,0.355021145260182,-4.42104600192432));
#10272=CARTESIAN_POINT('Ctrl Pts',(82.9963763800366,0.480458980621974,-4.4094964009439));
#10273=CARTESIAN_POINT('Ctrl Pts',(83.0015360391351,0.605031145700445,-4.39262062142151));
#10274=CARTESIAN_POINT('Ctrl Pts',(83.0063406759549,0.721031834823586,-4.37690601894306));
#10275=CARTESIAN_POINT('Ctrl Pts',(83.0112117514418,0.836282318339334,-4.35657281110158));
#10276=CARTESIAN_POINT('Ctrl Pts',(83.0162215122836,0.950372167218369,-4.33168733254973));
#10277=CARTESIAN_POINT('Ctrl Pts',(83.0165996648668,0.958984029627877,-4.32980889797041));
#10278=CARTESIAN_POINT('Ctrl Pts',(83.0169786076386,0.967589302089159,-4.32790453468976));
#10279=CARTESIAN_POINT('Ctrl Pts',(83.017358371671,0.976187819452551,-4.3259742753369));
#10280=CARTESIAN_POINT('Ctrl Pts',(83.020341280886,1.04372606555874,-4.31081278577855));
#10281=CARTESIAN_POINT('Ctrl Pts',(83.0233749977415,1.11084583174612,-4.29405393857436));
#10282=CARTESIAN_POINT('Ctrl Pts',(83.0264749356101,1.17746184370479,-4.27571908021852));
#10283=CARTESIAN_POINT('Ctrl Pts',(83.0264771251977,1.1775088967755,-4.27570612970766));
#10284=CARTESIAN_POINT('Ctrl Pts',(83.0264793148184,1.17755594959518,-4.27569317841065));
#10285=CARTESIAN_POINT('Ctrl Pts',(83.0264815044721,1.17760300216381,-4.27568022632754));
#10286=CARTESIAN_POINT('Ctrl Pts',(83.031631555246,1.28827032652172,-4.24521701412813));
#10287=CARTESIAN_POINT('Ctrl Pts',(83.0369750667503,1.39786167467843,-4.21030931034651));
#10288=CARTESIAN_POINT('Ctrl Pts',(83.0424357424794,1.50601219890857,-4.17108757267222));
#10289=CARTESIAN_POINT('Ctrl Pts',(83.0430131410074,1.51744777146085,-4.16694036182888));
#10290=CARTESIAN_POINT('Ctrl Pts',(83.0435918494819,1.52886720783642,-4.16274495782363));
#10291=CARTESIAN_POINT('Ctrl Pts',(83.0441717777059,1.54027005805773,-4.15850154327633));
#10292=CARTESIAN_POINT('Ctrl Pts',(83.0502290459922,1.65937121602083,-4.11417967843622));
#10293=CARTESIAN_POINT('Ctrl Pts',(83.0564188321494,1.77666664557797,-4.06461532858667));
#10294=CARTESIAN_POINT('Ctrl Pts',(83.0626487687321,1.89169347240627,-4.01002655004524));
#10295=CARTESIAN_POINT('Ctrl Pts',(83.068872772623,2.00661076060745,-3.9554897557237));
#10296=CARTESIAN_POINT('Ctrl Pts',(83.0751364884606,2.11926396248689,-3.89593843265172));
#10297=CARTESIAN_POINT('Ctrl Pts',(83.0813650127668,2.22921934865866,-3.83162264812522));
#10298=CARTESIAN_POINT('Ctrl Pts',(83.0873458487568,2.33480216387975,-3.76986449484245));
#10299=CARTESIAN_POINT('Ctrl Pts',(83.0932938490061,2.43789893180415,-3.70371211631604));
#10300=CARTESIAN_POINT('Ctrl Pts',(83.0991143652774,2.5380963922071,-3.63334847875165));
#10301=CARTESIAN_POINT('Ctrl Pts',(83.0996646519468,2.54756931938391,-3.6266961183838));
#10302=CARTESIAN_POINT('Ctrl Pts',(83.1002137991261,2.55701630012658,-3.62000613859655));
#10303=CARTESIAN_POINT('Ctrl Pts',(83.1007617268327,2.56643696581559,-3.61327870839512));
#10304=CARTESIAN_POINT('Ctrl Pts',(83.1050766073558,2.64062384559076,-3.56030081150069));
#10305=CARTESIAN_POINT('Ctrl Pts',(83.1092212503589,2.7130810149356,-3.50486908319631));
#10306=CARTESIAN_POINT('Ctrl Pts',(83.1133169435521,2.78379252150318,-3.4472891530527));
#10307=CARTESIAN_POINT('Ctrl Pts',(83.1149440208849,2.81188375882832,-3.42441463713097));
#10308=CARTESIAN_POINT('Ctrl Pts',(83.1165633729672,2.83969995819367,-3.40120074459727));
#10309=CARTESIAN_POINT('Ctrl Pts',(83.1181826040973,2.86724187719823,-3.37766518050719));
#10310=CARTESIAN_POINT('Ctrl Pts',(83.1238769429428,2.96409835207831,-3.29489782607189));
#10311=CARTESIAN_POINT('Ctrl Pts',(83.1295698325491,3.05756544207097,-3.20815179462532));
#10312=CARTESIAN_POINT('Ctrl Pts',(83.1352635643397,3.14733049837667,-3.11773076315744));
#10313=CARTESIAN_POINT('Ctrl Pts',(83.1409577238474,3.23710229789627,-3.02730293919834));
#10314=CARTESIAN_POINT('Ctrl Pts',(83.1466527721168,3.32317236319105,-2.93319848395593));
#10315=CARTESIAN_POINT('Ctrl Pts',(83.15234916326,3.40520966066485,-2.83571279856705));
#10316=CARTESIAN_POINT('Ctrl Pts',(83.156465764087,3.46449540810214,-2.76526299219011));
#10317=CARTESIAN_POINT('Ctrl Pts',(83.1603823538859,3.52140497973347,-2.69282752856406));
#10318=CARTESIAN_POINT('Ctrl Pts',(83.1642220955801,3.57594577686112,-2.61868992215394));
#10319=CARTESIAN_POINT('Ctrl Pts',(83.1656972154139,3.59689880391248,-2.59020835689558));
#10320=CARTESIAN_POINT('Ctrl Pts',(83.1671609934016,3.61750259350637,-2.56147516766554));
#10321=CARTESIAN_POINT('Ctrl Pts',(83.1686204127657,3.63775885406154,-2.53250484177084));
#10322=CARTESIAN_POINT('Ctrl Pts',(83.1738842292335,3.71081889458932,-2.42801501364069));
#10323=CARTESIAN_POINT('Ctrl Pts',(83.1790915795336,3.77935744318782,-2.32044082006187));
#10324=CARTESIAN_POINT('Ctrl Pts',(83.1843073977264,3.84309018161013,-2.21019936344676));
#10325=CARTESIAN_POINT('Ctrl Pts',(83.1895263928587,3.90686173945572,-2.09989075908509));
#10326=CARTESIAN_POINT('Ctrl Pts',(83.1947542364531,3.96582124515078,-1.98691151111031));
#10327=CARTESIAN_POINT('Ctrl Pts',(83.2000719246885,4.01971677939873,-1.87171061619713));
#10328=CARTESIAN_POINT('Ctrl Pts',(83.2049704710994,4.06936425103758,-1.76558989130256));
#10329=CARTESIAN_POINT('Ctrl Pts',(83.209945708905,4.11471474761423,-1.65758342461459));
#10330=CARTESIAN_POINT('Ctrl Pts',(83.2150681294169,4.15560070766259,-1.54806904063664));
#10331=CARTESIAN_POINT('Ctrl Pts',(83.2155141276777,4.15916056125742,-1.53853385611296));
#10332=CARTESIAN_POINT('Ctrl Pts',(83.2159612417034,4.16268659683867,-1.52898722160007));
#10333=CARTESIAN_POINT('Ctrl Pts',(83.2164095180213,4.16617871895642,-1.51942937543462));
#10334=CARTESIAN_POINT('Ctrl Pts',(83.2184084439692,4.18175057327004,-1.4768096207348));
#10335=CARTESIAN_POINT('Ctrl Pts',(83.2204305259555,4.19664788204346,-1.43396768820987));
#10336=CARTESIAN_POINT('Ctrl Pts',(83.2224799502902,4.2108624193871,-1.39092663162212));
#10337=CARTESIAN_POINT('Ctrl Pts',(83.2224818919627,4.21087588657161,-1.39088585352034));
#10338=CARTESIAN_POINT('Ctrl Pts',(83.2224838336597,4.21088935314335,-1.39084507523976));
#10339=CARTESIAN_POINT('Ctrl Pts',(83.2224857753812,4.21090281910232,-1.39080429678043));
#10340=CARTESIAN_POINT('Ctrl Pts',(83.2276958762136,4.24703519050223,-1.28138598944583));
#10341=CARTESIAN_POINT('Ctrl Pts',(83.2330927463868,4.27884346901629,-1.17038633843429));
#10342=CARTESIAN_POINT('Ctrl Pts',(83.238599482485,4.30623236297333,-1.05818515621962));
#10343=CARTESIAN_POINT('Ctrl Pts',(83.2391478689658,4.30895987685862,-1.04701163884735));
#10344=CARTESIAN_POINT('Ctrl Pts',(83.2396973449987,4.31164357857737,-1.03582624554528));
#10345=CARTESIAN_POINT('Ctrl Pts',(83.2402478346343,4.31428338468635,-1.02462937754755));
#10346=CARTESIAN_POINT('Ctrl Pts',(83.2463188982337,4.34339643194308,-0.90114494964345));
#10347=CARTESIAN_POINT('Ctrl Pts',(83.2525127122266,4.367168791287,-0.776259208809224));
#10348=CARTESIAN_POINT('Ctrl Pts',(83.2587383288107,4.38552444664463,-0.650475198184107));
#10349=CARTESIAN_POINT('Ctrl Pts',(83.2649580273905,4.40386265331336,-0.524810756488961));
#10350=CARTESIAN_POINT('Ctrl Pts',(83.2712091204897,4.41679482015103,-0.398249774132754));
#10351=CARTESIAN_POINT('Ctrl Pts',(83.2774183828953,4.4242873067542,-0.271289330281206));
#10352=CARTESIAN_POINT('Ctrl Pts',(83.2818665938466,4.42965479789635,-0.180337007791962));
#10353=CARTESIAN_POINT('Ctrl Pts',(83.2862932319342,4.43223067893641,-0.0891765403184688));
#10354=CARTESIAN_POINT('Ctrl Pts',(83.2905748263073,4.43183580562401,0.00200120831765594));
#10355=CARTESIAN_POINT('Ctrl Pts',(83.2922657104634,4.43167986254079,0.0380090589267377));
#10356=CARTESIAN_POINT('Ctrl Pts',(83.2939339734225,4.43106060173415,0.0740190327286194));
#10357=CARTESIAN_POINT('Ctrl Pts',(83.2955720103559,4.42996711655931,0.110017136420428));
#10358=CARTESIAN_POINT('Ctrl Pts',(83.3013557983644,4.42610610078323,0.237123794527655));
#10359=CARTESIAN_POINT('Ctrl Pts',(83.3070431808581,4.41681895720635,0.364089474368331));
#10360=CARTESIAN_POINT('Ctrl Pts',(83.3127292137339,4.40235937168851,0.490468223047512));
#10361=CARTESIAN_POINT('Ctrl Pts',(83.3202757972191,4.38316840468998,0.658199890889831));
#10362=CARTESIAN_POINT('Ctrl Pts',(83.3278200867937,4.3548679440162,0.824908498874133));
#10363=CARTESIAN_POINT('Ctrl Pts',(83.3353674090675,4.31762806162275,0.989594993068796));
#10364=CARTESIAN_POINT('Ctrl Pts',(83.3391920019019,4.29875681402142,1.07304959627369));
#10365=CARTESIAN_POINT('Ctrl Pts',(83.3430173561456,4.27758922004229,1.15598442351761));
#10366=CARTESIAN_POINT('Ctrl Pts',(83.3468440873736,4.25414314863876,1.23826639036087));
#10367=CARTESIAN_POINT('Ctrl Pts',(83.3517492151144,4.22408982939495,1.34373592404053));
#10368=CARTESIAN_POINT('Ctrl Pts',(83.3565356218405,4.19008965765042,1.44807887305938));
#10369=CARTESIAN_POINT('Ctrl Pts',(83.3611065242648,4.15204113187027,1.55088410347697));
#10370=CARTESIAN_POINT('Ctrl Pts',(83.3618388982381,4.14594479740122,1.567356096989));
#10371=CARTESIAN_POINT('Ctrl Pts',(83.362565739757,4.13974457730305,1.58378851468944));
#10372=CARTESIAN_POINT('Ctrl Pts',(83.3632866507204,4.13344010795501,1.60017955307763));
#10373=CARTESIAN_POINT('Ctrl Pts',(83.3685125371654,4.08773898454253,1.71899825563343));
#10374=CARTESIAN_POINT('Ctrl Pts',(83.3736802157154,4.03696913488963,1.8357987771688));
#10375=CARTESIAN_POINT('Ctrl Pts',(83.3788545764085,3.98131696754136,1.95011384795414));
#10376=CARTESIAN_POINT('Ctrl Pts',(83.3840321159857,3.92563061011647,2.06449914854751));
#10377=CARTESIAN_POINT('Ctrl Pts',(83.3892167134998,3.86505561520871,2.17639569603508));
#10378=CARTESIAN_POINT('Ctrl Pts',(83.3944892480764,3.79982286445714,2.28534536985133));
#10379=CARTESIAN_POINT('Ctrl Pts',(83.3993493524282,3.73969277499033,2.38577274043547));
#10380=CARTESIAN_POINT('Ctrl Pts',(83.4042846234623,3.67560478451595,2.48369665225706));
#10381=CARTESIAN_POINT('Ctrl Pts',(83.4093655796607,3.60777834532099,2.57876776006166));
#10382=CARTESIAN_POINT('Ctrl Pts',(83.4098046666016,3.60191690851023,2.58698363129919));
#10383=CARTESIAN_POINT('Ctrl Pts',(83.4102448415338,3.5960275520837,2.59517822973848));
#10384=CARTESIAN_POINT('Ctrl Pts',(83.4106861499687,3.59011041702327,2.60335134822733));
#10385=CARTESIAN_POINT('Ctrl Pts',(83.4130537171506,3.55836569230572,2.64719915529321));
#10386=CARTESIAN_POINT('Ctrl Pts',(83.4154539753355,3.52582211620615,2.69042785635404));
#10387=CARTESIAN_POINT('Ctrl Pts',(83.4178940510447,3.49250453772734,2.73300404509958));
#10388=CARTESIAN_POINT('Ctrl Pts',(83.4178960990468,3.49247657364914,2.73303978010571));
#10389=CARTESIAN_POINT('Ctrl Pts',(83.4178981470768,3.49244860902571,2.73307551465235));
#10390=CARTESIAN_POINT('Ctrl Pts',(83.4179001951349,3.49242064385706,2.73311124873948));
#10391=CARTESIAN_POINT('Ctrl Pts',(83.4230804538993,3.42168690417833,2.82349531361935));
#10392=CARTESIAN_POINT('Ctrl Pts',(83.4284505832191,3.34726193598441,2.91118426735303));
#10393=CARTESIAN_POINT('Ctrl Pts',(83.4339335812588,3.26940588398292,2.9958897134484));
#10394=CARTESIAN_POINT('Ctrl Pts',(83.4344900909845,3.26150370166652,3.00448709105785));
#10395=CARTESIAN_POINT('Ctrl Pts',(83.4350477634512,3.25356621653918,3.01305372383549));
#10396=CARTESIAN_POINT('Ctrl Pts',(83.4356065181459,3.24559372995324,3.02158930431373));
#10397=CARTESIAN_POINT('Ctrl Pts',(83.4416628908757,3.15917951132197,3.1141069284753));
#10398=CARTESIAN_POINT('Ctrl Pts',(83.4478458747289,3.06864739174935,3.20297803546822));
#10399=CARTESIAN_POINT('Ctrl Pts',(83.4540637428815,2.97437175577744,3.28786046013636));
#10400=CARTESIAN_POINT('Ctrl Pts',(83.4602754787236,2.88018909821294,3.37265917035822));
#10401=CARTESIAN_POINT('Ctrl Pts',(83.4665216800954,2.78227053048892,3.45347735854507));
#10402=CARTESIAN_POINT('Ctrl Pts',(83.472728267662,2.68100906535056,3.53001146314587));
#10403=CARTESIAN_POINT('Ctrl Pts',(83.4774236798418,2.60440266744516,3.58791110011411));
#10404=CARTESIAN_POINT('Ctrl Pts',(83.4820963018083,2.52588060915895,3.64336056465543));
#10405=CARTESIAN_POINT('Ctrl Pts',(83.4866286167864,2.44553776480205,3.69610140141218));
#10406=CARTESIAN_POINT('Ctrl Pts',(83.4880828915604,2.41975831823126,3.71302424742482));
#10407=CARTESIAN_POINT('Ctrl Pts',(83.4895227208511,2.39379174784691,3.72966800614239));
#10408=CARTESIAN_POINT('Ctrl Pts',(83.4909442224484,2.36764216970578,3.74602356322536));
#10409=CARTESIAN_POINT('Ctrl Pts',(83.4958650556628,2.27711978626616,3.80264183835173));
#10410=CARTESIAN_POINT('Ctrl Pts',(83.500662889532,2.18449736086475,3.85594589781447));
#10411=CARTESIAN_POINT('Ctrl Pts',(83.505440332829,2.09013217084792,3.90597666055246));
#10412=CARTESIAN_POINT('Ctrl Pts',(83.5063418383544,2.07232542047616,3.9154174861665));
#10413=CARTESIAN_POINT('Ctrl Pts',(83.5072426178155,2.05445647939991,3.92474182120197));
#10414=CARTESIAN_POINT('Ctrl Pts',(83.5081433606626,2.03652755806437,3.93395002496193));
#10415=CARTESIAN_POINT('Ctrl Pts',(83.5156887938591,1.88633876816063,4.01108623154202));
#10416=CARTESIAN_POINT('Ctrl Pts',(83.5232317390843,1.73194090282254,4.08007809689432));
#10417=CARTESIAN_POINT('Ctrl Pts',(83.5307775529328,1.57426266678588,4.1405149697427));
#10418=CARTESIAN_POINT('Ctrl Pts',(83.5345789459057,1.49482830085911,4.17096156017889));
#10419=CARTESIAN_POINT('Ctrl Pts',(83.538381051415,1.41456137295648,4.19923609301629));
#10420=CARTESIAN_POINT('Ctrl Pts',(83.5421844836819,1.33358065191831,4.22528092553794));
#10421=CARTESIAN_POINT('Ctrl Pts',(83.5471073281589,1.22876598260772,4.25899117747211));
#10422=CARTESIAN_POINT('Ctrl Pts',(83.5519120286095,1.12268776988625,4.28876818841022));
#10423=CARTESIAN_POINT('Ctrl Pts',(83.556502202349,1.01563498595979,4.31429907462853));
#10424=CARTESIAN_POINT('Ctrl Pts',(83.5572066933098,0.999204732359207,4.31821750551682));
#10425=CARTESIAN_POINT('Ctrl Pts',(83.5579061309835,0.982751620683477,4.32203589941005));
#10426=CARTESIAN_POINT('Ctrl Pts',(83.5586001669221,0.966276803372248,4.32575310922017));
#10427=CARTESIAN_POINT('Ctrl Pts',(83.5638217887403,0.842327508043682,4.35371976450071));
#10428=CARTESIAN_POINT('Ctrl Pts',(83.5689828774853,0.717244017525123,4.37637234041289));
#10429=CARTESIAN_POINT('Ctrl Pts',(83.574147593184,0.591516394640054,4.39360678407597));
#10430=CARTESIAN_POINT('Ctrl Pts',(83.5793154218535,0.465712990929349,4.41085161559448));
#10431=CARTESIAN_POINT('Ctrl Pts',(83.5844872421536,0.339264707288376,4.42267138590536));
#10432=CARTESIAN_POINT('Ctrl Pts',(83.5897434241407,0.212678499269937,4.429003912549));
#10433=CARTESIAN_POINT('Ctrl Pts',(83.5946043131319,0.0956122510871442,
4.4348601993222));
#10434=CARTESIAN_POINT('Ctrl Pts',(83.5995377961836,-0.0215724676693285,
4.43602349133232));
#10435=CARTESIAN_POINT('Ctrl Pts',(83.6046149580464,-0.138461181276436,
4.43248217517797));
#10436=CARTESIAN_POINT('Ctrl Pts',(83.6050357345095,-0.148148487063251,
4.43218868394672));
#10437=CARTESIAN_POINT('Ctrl Pts',(83.6054574978282,-0.157833784798538,
4.43186289506993));
#10438=CARTESIAN_POINT('Ctrl Pts',(83.6058802884664,-0.1675168523186,4.43150481028875));
#10439=CARTESIAN_POINT('Ctrl Pts',(83.6083705427704,-0.224550519560011,
4.42939567615212));
#10440=CARTESIAN_POINT('Ctrl Pts',(83.6108965182637,-0.281505603001958,
4.42616618672832));
#10441=CARTESIAN_POINT('Ctrl Pts',(83.6134666278495,-0.338333304651339,
4.42181886367226));
#10442=CARTESIAN_POINT('Ctrl Pts',(83.6134686787691,-0.338378652541717,
4.42181539455555));
#10443=CARTESIAN_POINT('Ctrl Pts',(83.6134707297169,-0.338424000351126,
4.42181192472713));
#10444=CARTESIAN_POINT('Ctrl Pts',(83.6134727806927,-0.338469348079556,
4.42180845418703));
#10445=CARTESIAN_POINT('Ctrl Pts',(83.618654874038,-0.453047081791832,4.41303962202268));
#10446=CARTESIAN_POINT('Ctrl Pts',(83.6240267635337,-0.567422948792048,
4.39969405719048));
#10447=CARTESIAN_POINT('Ctrl Pts',(83.6295116449866,-0.681212096767725,
4.38182930509884));
#10448=CARTESIAN_POINT('Ctrl Pts',(83.6300706981457,-0.692810192950719,
4.3800084186898));
#10449=CARTESIAN_POINT('Ctrl Pts',(83.6306309251727,-0.704402161603934,
4.37814061365625));
#10450=CARTESIAN_POINT('Ctrl Pts',(83.6311922447393,-0.715987573789082,
4.37622597240999));
#10451=CARTESIAN_POINT('Ctrl Pts',(83.6372533034713,-0.841085410874153,
4.35555191482162));
#10452=CARTESIAN_POINT('Ctrl Pts',(83.6434412084401,-0.96542337207803,4.32941315273088));
#10453=CARTESIAN_POINT('Ctrl Pts',(83.649664316664,-1.08850789870529,4.29793296106795));
#10454=CARTESIAN_POINT('Ctrl Pts',(83.6558814031489,-1.21147332361096,4.26648323095146));
#10455=CARTESIAN_POINT('Ctrl Pts',(83.6621332726753,-1.33318786235633,4.22970275874476));
#10456=CARTESIAN_POINT('Ctrl Pts',(83.6683459091601,-1.45317992705797,4.18775171601595));
#10457=CARTESIAN_POINT('Ctrl Pts',(83.6731578198372,-1.54611810213333,4.15525912274806));
#10458=CARTESIAN_POINT('Ctrl Pts',(83.6779460695833,-1.63802567327674,4.11966361603014));
#10459=CARTESIAN_POINT('Ctrl Pts',(83.6825958502752,-1.72862303737288,4.08091454301838));
#10460=CARTESIAN_POINT('Ctrl Pts',(83.6839450610236,-1.75491136052506,4.06967085879707));
#10461=CARTESIAN_POINT('Ctrl Pts',(83.685282613146,-1.78108906197937,4.05816178987407));
#10462=CARTESIAN_POINT('Ctrl Pts',(83.6866057017605,-1.80714857123362,4.04638645852495));
#10463=CARTESIAN_POINT('Ctrl Pts',(83.6914041439244,-1.90165852817018,4.0036808938168));
#10464=CARTESIAN_POINT('Ctrl Pts',(83.6960718155216,-1.99465230072675,3.95756905734555));
#10465=CARTESIAN_POINT('Ctrl Pts',(83.7007146286701,-2.08598548365827,3.90836441317301));
#10466=CARTESIAN_POINT('Ctrl Pts',(83.7017617439562,-2.10658428204085,3.89726706046652));
#10467=CARTESIAN_POINT('Ctrl Pts',(83.7028075947953,-2.1270987954403,3.8860122855028));
#10468=CARTESIAN_POINT('Ctrl Pts',(83.7038533962134,-2.1475276796128,3.87460349311657));
#10469=CARTESIAN_POINT('Ctrl Pts',(83.7114039453886,-2.29502154591708,3.79223350733086));
#10470=CARTESIAN_POINT('Ctrl Pts',(83.7189520000807,-2.43805615563127,3.70183762496549));
#10471=CARTESIAN_POINT('Ctrl Pts',(83.7265029116128,-2.57577454065322,3.603962383649));
#10472=CARTESIAN_POINT('Ctrl Pts',(83.7303166368923,-2.64533171718342,3.55452871190574));
#10473=CARTESIAN_POINT('Ctrl Pts',(83.7341310752323,-2.71353203111865,3.50318657492858));
#10474=CARTESIAN_POINT('Ctrl Pts',(83.7379468442458,-2.78026072840528,3.45000355426256));
#10475=CARTESIAN_POINT('Ctrl Pts',(83.7436340194881,-2.87971585627676,3.37073744633586));
#10476=CARTESIAN_POINT('Ctrl Pts',(83.7491229268731,-2.97568597598866,3.28710709185555));
#10477=CARTESIAN_POINT('Ctrl Pts',(83.7543517004372,-3.06761895138763,3.19933279850464));
#10478=CARTESIAN_POINT('Ctrl Pts',(83.7595860249966,-3.15964952510658,3.11146532179344));
#10479=CARTESIAN_POINT('Ctrl Pts',(83.7647608101047,-3.24787155568025,3.01970019803276));
#10480=CARTESIAN_POINT('Ctrl Pts',(83.7699403890791,-3.33192600747476,2.92438887205071));
#10481=CARTESIAN_POINT('Ctrl Pts',(83.7751231036246,-3.41603134346466,2.829019847279));
#10482=CARTESIAN_POINT('Ctrl Pts',(83.7803109808668,-3.49596370603902,2.73010012777394));
#10483=CARTESIAN_POINT('Ctrl Pts',(83.7855845286649,-3.57138955912243,2.62801851725546));
#10484=CARTESIAN_POINT('Ctrl Pts',(83.7904563696584,-3.64106992935743,2.533712863102));
#10485=CARTESIAN_POINT('Ctrl Pts',(83.7954017729062,-3.70690444270405,2.43670821705469));
#10486=CARTESIAN_POINT('Ctrl Pts',(83.8004916423735,-3.76865384235248,2.33734320296745));
#10487=CARTESIAN_POINT('Ctrl Pts',(83.8009191948214,-3.77384083332494,2.32899647516146));
#10488=CARTESIAN_POINT('Ctrl Pts',(83.8013477666393,-3.77899902712594,2.3206330799814));
#10489=CARTESIAN_POINT('Ctrl Pts',(83.8017773998531,-3.78412829715226,2.31225321102945));
#10490=CARTESIAN_POINT('Ctrl Pts',(83.8041810383647,-3.81282466087439,2.26537095173032));
#10491=CARTESIAN_POINT('Ctrl Pts',(83.8066179712436,-3.8406151563232,2.21797404828616));
#10492=CARTESIAN_POINT('Ctrl Pts',(83.8090956800703,-3.86747750675075,2.17009996787264));
#10493=CARTESIAN_POINT('Ctrl Pts',(83.8090977039212,-3.86749944855063,2.17006086319733));
#10494=CARTESIAN_POINT('Ctrl Pts',(83.8090997277993,-3.86752138973141,2.17002175820357));
#10495=CARTESIAN_POINT('Ctrl Pts',(83.8091017517046,-3.8675433302931,2.16998265289143));
#10496=CARTESIAN_POINT('Ctrl Pts',(83.8144007795553,-3.92498853209468,2.06759637036372));
#10497=CARTESIAN_POINT('Ctrl Pts',(83.8198957562386,-3.97832517195201,1.96276873835478));
#10498=CARTESIAN_POINT('Ctrl Pts',(83.825505383901,-4.02739117448023,1.85586145227348));
#10499=CARTESIAN_POINT('Ctrl Pts',(83.8261913020303,-4.03339072787186,1.84278934658422));
#10500=CARTESIAN_POINT('Ctrl Pts',(83.8268789343311,-4.03932643526781,1.82968621130896));
#10501=CARTESIAN_POINT('Ctrl Pts',(83.8275681321777,-4.04519800591419,1.81655276077925));
#10502=CARTESIAN_POINT('Ctrl Pts',(83.8338838104617,-4.09900396512889,1.69620031232743));
#10503=CARTESIAN_POINT('Ctrl Pts',(83.8403303453004,-4.14742402367748,1.57329554968749));
#10504=CARTESIAN_POINT('Ctrl Pts',(83.8468067626538,-4.19027938554954,1.44835441049137));
#10505=CARTESIAN_POINT('Ctrl Pts',(83.8532704385826,-4.23305043562794,1.3236590751127));
#10506=CARTESIAN_POINT('Ctrl Pts',(83.8597634953365,-4.2702791213177,1.19693534424601));
#10507=CARTESIAN_POINT('Ctrl Pts',(83.8662062977059,-4.30182808985253,1.06869775645993));
#10508=CARTESIAN_POINT('Ctrl Pts',(83.8706801815884,-4.32373570299136,0.979649537340729));
#10509=CARTESIAN_POINT('Ctrl Pts',(83.8751297259372,-4.34290503282981,0.889868301763519));
#10510=CARTESIAN_POINT('Ctrl Pts',(83.8794335881289,-4.35912518117283,0.799504371769359));
#10511=CARTESIAN_POINT('Ctrl Pts',(83.8813204430654,-4.3662362515575,0.759887948242621));
#10512=CARTESIAN_POINT('Ctrl Pts',(83.8831792974447,-4.37278033297821,0.720160187088544));
#10513=CARTESIAN_POINT('Ctrl Pts',(83.8849999264898,-4.37873913709929,0.680336875005218));
#10514=CARTESIAN_POINT('Ctrl Pts',(83.8909649371895,-4.39826224118045,0.549861925525245));
#10515=CARTESIAN_POINT('Ctrl Pts',(83.8968658543233,-4.4120960442704,0.418457158923947));
#10516=CARTESIAN_POINT('Ctrl Pts',(83.9027691917311,-4.4203396281389,0.286618145884316));
#10517=CARTESIAN_POINT('Ctrl Pts',(83.907044634625,-4.42630997501838,0.191134840000573));
#10518=CARTESIAN_POINT('Ctrl Pts',(83.9113213748735,-4.42934795132635,0.0954213214250343));
#10519=CARTESIAN_POINT('Ctrl Pts',(83.915600810406,-4.42944218562652,-0.000347422039578667));
#10520=CARTESIAN_POINT('',(85.1613954767416,-4.43439065261444,-0.00220057529882202));
#10521=CARTESIAN_POINT('Ctrl Pts',(83.9156030730062,-4.42944223517521,-0.000398056376253822));
#10522=CARTESIAN_POINT('Ctrl Pts',(83.9200220896795,-4.42945985862297,-0.100320665778061));
#10523=CARTESIAN_POINT('Ctrl Pts',(83.9245029427185,-4.42639348513736,-0.200087969978499));
#10524=CARTESIAN_POINT('Ctrl Pts',(83.9289760356259,-4.42011577234908,-0.299621035218978));
#10525=CARTESIAN_POINT('Ctrl Pts',(83.9305230564219,-4.41794462311603,-0.334044581747511));
#10526=CARTESIAN_POINT('Ctrl Pts',(83.9320691490095,-4.41538902195064,-0.368439800463256));
#10527=CARTESIAN_POINT('Ctrl Pts',(83.9336114343194,-4.4124426794653,-0.402802392015783));
#10528=CARTESIAN_POINT('Ctrl Pts',(83.9399260209631,-4.40037945433718,-0.543493326605526));
#10529=CARTESIAN_POINT('Ctrl Pts',(83.9459499749625,-4.38139419249402,-0.683482294095519));
#10530=CARTESIAN_POINT('Ctrl Pts',(83.9517310700353,-4.35555705311141,-0.822055333667062));
#10531=CARTESIAN_POINT('Ctrl Pts',(83.9572489548599,-4.33089626523016,-0.954319214909025));
#10532=CARTESIAN_POINT('Ctrl Pts',(83.962705971755,-4.30026642860534,-1.08534392858136));
#10533=CARTESIAN_POINT('Ctrl Pts',(83.9681825322541,-4.26378442005296,-1.21458324295616));
#10534=CARTESIAN_POINT('Ctrl Pts',(83.973361322082,-4.22928600543357,-1.33679557800421));
#10535=CARTESIAN_POINT('Ctrl Pts',(83.9785580193129,-4.18955396851155,-1.45741185058128));
#10536=CARTESIAN_POINT('Ctrl Pts',(83.9838564405357,-4.14472505692022,-1.57596796994945));
#10537=CARTESIAN_POINT('Ctrl Pts',(83.9841690471093,-4.14208015349308,-1.58296277475942));
#10538=CARTESIAN_POINT('Ctrl Pts',(83.9844820077835,-4.13941750629901,-1.58995042318379));
#10539=CARTESIAN_POINT('Ctrl Pts',(83.9847953397724,-4.13673714269204,-1.59693082553478));
#10540=CARTESIAN_POINT('Ctrl Pts',(83.989745650979,-4.09439025673095,-1.70721373698422));
#10541=CARTESIAN_POINT('Ctrl Pts',(83.994789192224,-4.04762128275976,-1.81568482447509));
#10542=CARTESIAN_POINT('Ctrl Pts',(84.0000005781829,-3.99657730699651,-1.92196719207186));
#10543=CARTESIAN_POINT('Ctrl Pts',(84.0007224333611,-3.98950695018371,-1.93668889528134));
#10544=CARTESIAN_POINT('Ctrl Pts',(84.0014475088764,-3.98235457773494,-1.95136868637714));
#10545=CARTESIAN_POINT('Ctrl Pts',(84.0021760030253,-3.97512058473301,-1.96600564259331));
#10546=CARTESIAN_POINT('Ctrl Pts',(84.0029981870553,-3.96695624528217,-1.98252502256009));
#10547=CARTESIAN_POINT('Ctrl Pts',(84.003824730455,-3.95868802532439,-1.99898971458215));
#10548=CARTESIAN_POINT('Ctrl Pts',(84.0046559199584,-3.9503165789104,-2.01539830187999));
#10549=CARTESIAN_POINT('Ctrl Pts',(84.0046579578214,-3.95029605427527,-2.01543853151902));
#10550=CARTESIAN_POINT('Ctrl Pts',(84.0046599957124,-3.95027552901963,-2.01547876082083));
#10551=CARTESIAN_POINT('Ctrl Pts',(84.0046620336313,-3.95025500314353,-2.01551898978539));
#10552=CARTESIAN_POINT('Ctrl Pts',(84.0098464822127,-3.89803734672897,-2.11786113776804));
#10553=CARTESIAN_POINT('Ctrl Pts',(84.0152204254087,-3.84167465055871,-2.21825612911228));
#10554=CARTESIAN_POINT('Ctrl Pts',(84.020706973181,-3.78136802300308,-2.31637084667125));
#10555=CARTESIAN_POINT('Ctrl Pts',(84.021263903114,-3.77524640200608,-2.32633030120334));
#10556=CARTESIAN_POINT('Ctrl Pts',(84.0218219933164,-3.76908418364762,-2.33626624232669));
#10557=CARTESIAN_POINT('Ctrl Pts',(84.0223811633663,-3.76288160597131,-2.3461783102358));
#10558=CARTESIAN_POINT('Ctrl Pts',(84.0284415357854,-3.69565709942856,-2.45360685184891));
#10559=CARTESIAN_POINT('Ctrl Pts',(84.0346282174866,-3.62368643149239,-2.55823383882937));
#10560=CARTESIAN_POINT('Ctrl Pts',(84.0408496095882,-3.54727283849583,-2.65965152486281));
#10561=CARTESIAN_POINT('Ctrl Pts',(84.0470649488748,-3.4709335885614,-2.76097054126119));
#10562=CARTESIAN_POINT('Ctrl Pts',(84.0533145802337,-3.39016033354804,-2.8590867479529));
#10563=CARTESIAN_POINT('Ctrl Pts',(84.0595245500108,-3.30528192202576,-2.95362680933311));
#10564=CARTESIAN_POINT('Ctrl Pts',(84.0642453959957,-3.24075698508966,-3.02549657443695));
#10565=CARTESIAN_POINT('Ctrl Pts',(84.0689432014021,-3.17385757186749,-3.09530178468054));
#10566=CARTESIAN_POINT('Ctrl Pts',(84.0735010891228,-3.10463126550535,-3.16276943169823));
#10567=CARTESIAN_POINT('Ctrl Pts',(84.0749344687681,-3.08286074711311,-3.18398688106778));
#10568=CARTESIAN_POINT('Ctrl Pts',(84.0763540105883,-3.06086037940469,-3.20497287834147));
#10569=CARTESIAN_POINT('Ctrl Pts',(84.077756079434,-3.03863244229489,-3.22571822680655));
#10570=CARTESIAN_POINT('Ctrl Pts',(84.0826619466766,-2.96085644087079,-3.298306620583));
#10571=CARTESIAN_POINT('Ctrl Pts',(84.0874437688791,-2.88040415007025,-3.36805936072332));
#10572=CARTESIAN_POINT('Ctrl Pts',(84.0922045774475,-2.79763216707804,-3.43495049127518));
#10573=CARTESIAN_POINT('Ctrl Pts',(84.0931287399803,-2.7815645675626,-3.44793531848348));
#10574=CARTESIAN_POINT('Ctrl Pts',(84.0940521106749,-2.76540943083509,-3.46081240846906));
#10575=CARTESIAN_POINT('Ctrl Pts',(84.0949754431863,-2.74916917906846,-3.47358170203163));
#10576=CARTESIAN_POINT('Ctrl Pts',(84.1025236857171,-2.61640513405698,-3.57797066654195));
#10577=CARTESIAN_POINT('Ctrl Pts',(84.1100694581678,-2.47795358470528,-3.67516035798));
#10578=CARTESIAN_POINT('Ctrl Pts',(84.1176181112967,-2.33464800299958,-3.76457020605654));
#10579=CARTESIAN_POINT('Ctrl Pts',(84.1214282800525,-2.26231477472148,-3.80969966210601));
#10580=CARTESIAN_POINT('Ctrl Pts',(84.1252391669181,-2.18874467800358,-3.85284616832275));
#10581=CARTESIAN_POINT('Ctrl Pts',(84.1290513879722,-2.11404396154338,-3.89392997526874));
#10582=CARTESIAN_POINT('Ctrl Pts',(84.1343997316991,-2.00924282262703,-3.95156837504573));
#10583=CARTESIAN_POINT('Ctrl Pts',(84.1395900454753,-1.90207862838257,-4.00490400576711));
#10584=CARTESIAN_POINT('Ctrl Pts',(84.1445355063654,-1.79286940114767,-4.05352855524393));
#10585=CARTESIAN_POINT('Ctrl Pts',(84.1448461261242,-1.78601007204187,-4.05658261757847));
#10586=CARTESIAN_POINT('Ctrl Pts',(84.1451557799437,-1.77914269155742,-4.05961808944955));
#10587=CARTESIAN_POINT('Ctrl Pts',(84.1454644463109,-1.77226734507983,-4.06263486767839));
#10588=CARTESIAN_POINT('Ctrl Pts',(84.1506930242929,-1.6558041050483,-4.11373684023112));
#10589=CARTESIAN_POINT('Ctrl Pts',(84.1558618313948,-1.53721142653457,-4.15982835192703));
#10590=CARTESIAN_POINT('Ctrl Pts',(84.1610351961871,-1.41695144635677,-4.20071349901739));
#10591=CARTESIAN_POINT('Ctrl Pts',(84.1662116927519,-1.29661866503086,-4.24162339653298));
#10592=CARTESIAN_POINT('Ctrl Pts',(84.1713931150129,-1.17461651478789,-4.27732022802709));
#10593=CARTESIAN_POINT('Ctrl Pts',(84.1766599594209,-1.05143177192609,-4.30764600656593));
#10594=CARTESIAN_POINT('Ctrl Pts',(84.1815263579785,-0.937612944456394,
-4.33566607199942));
#10595=CARTESIAN_POINT('Ctrl Pts',(84.1864661287189,-0.82278399811288,-4.35910082126407));
#10596=CARTESIAN_POINT('Ctrl Pts',(84.1915502021094,-0.707349358148297,
-4.37785988037722));
#10597=CARTESIAN_POINT('Ctrl Pts',(84.1919764438846,-0.697671475456709,
-4.37943261429451));
#10598=CARTESIAN_POINT('Ctrl Pts',(84.1924036999512,-0.687989313361263,
-4.38097250404709));
#10599=CARTESIAN_POINT('Ctrl Pts',(84.1928320121081,-0.678303097849305,
-4.38247950761368));
#10600=CARTESIAN_POINT('Ctrl Pts',(84.1952646007355,-0.623290469050379,
-4.39103849824374));
#10601=CARTESIAN_POINT('Ctrl Pts',(84.1977313301607,-0.568148240667956,
-4.39853655272527));
#10602=CARTESIAN_POINT('Ctrl Pts',(84.2002399855675,-0.512921282444363,
-4.40496731133519));
#10603=CARTESIAN_POINT('Ctrl Pts',(84.2002420223226,-0.512876444166573,
-4.4049725324111));
#10604=CARTESIAN_POINT('Ctrl Pts',(84.2002440591053,-0.512831605832806,
-4.40497775278361));
#10605=CARTESIAN_POINT('Ctrl Pts',(84.2002460959157,-0.512786767443101,
-4.40498297245274));
#10606=CARTESIAN_POINT('Ctrl Pts',(84.2054311220285,-0.398643484480754,
-4.41827047396691));
#10607=CARTESIAN_POINT('Ctrl Pts',(84.2108055944895,-0.283822881198216,
-4.4270271922881));
#10608=CARTESIAN_POINT('Ctrl Pts',(84.2162926444345,-0.168713809015507,
-4.43123589822478));
#10609=CARTESIAN_POINT('Ctrl Pts',(84.2168497233916,-0.157027230155568,
-4.43166319185937));
#10610=CARTESIAN_POINT('Ctrl Pts',(84.2174079627475,-0.145337715089774,
-4.43204363065165));
#10611=CARTESIAN_POINT('Ctrl Pts',(84.2179672820597,-0.133645695587933,
-4.4323772133244));
#10612=CARTESIAN_POINT('Ctrl Pts',(84.2240283194387,-0.00694567704394078,
-4.43599206624319));
#10613=CARTESIAN_POINT('Ctrl Pts',(84.2302156387763,0.120053657973535,-4.4341017418951));
#10614=CARTESIAN_POINT('Ctrl Pts',(84.2364376599109,0.246844678988904,-4.42673266576923));
#10615=CARTESIAN_POINT('Ctrl Pts',(84.242653642254,0.373512642795672,-4.41937074171085));
#10616=CARTESIAN_POINT('Ctrl Pts',(84.2489039080635,0.499972749915472,-4.40654106651511));
#10617=CARTESIAN_POINT('Ctrl Pts',(84.2551145213253,0.62573182461737,-4.38831046061018));
#10618=CARTESIAN_POINT('Ctrl Pts',(84.2598428657655,0.721476350417396,-4.37443089985839));
#10619=CARTESIAN_POINT('Ctrl Pts',(84.2645481063376,0.816817457352416,-4.35742027862559));
#10620=CARTESIAN_POINT('Ctrl Pts',(84.2691135469234,0.911500643384384,-4.33716756098911));
#10621=CARTESIAN_POINT('Ctrl Pts',(84.2705404182196,0.941092687753812,-4.330837827654));
#10622=CARTESIAN_POINT('Ctrl Pts',(84.2719536338983,0.970620092880962,-4.32419149102998));
#10623=CARTESIAN_POINT('Ctrl Pts',(84.2733496313951,1.00007407902062,-4.3172254305111));
#10624=CARTESIAN_POINT('Ctrl Pts',(84.2782487153611,1.10343927240734,-4.29277888567797));
#10625=CARTESIAN_POINT('Ctrl Pts',(84.2830233214964,1.20593053517353,-4.26454360145908));
#10626=CARTESIAN_POINT('Ctrl Pts',(84.2877766640604,1.30732974394678,-4.23280178892722));
#10627=CARTESIAN_POINT('Ctrl Pts',(84.2887094415093,1.32722793012016,-4.2265728991471));
#10628=CARTESIAN_POINT('Ctrl Pts',(84.2896414001277,1.34708421448667,-4.22020892404134));
#10629=CARTESIAN_POINT('Ctrl Pts',(84.2905733198829,1.36689716823111,-4.21371191096212));
#10630=CARTESIAN_POINT('Ctrl Pts',(84.2981220981959,1.52738694721297,-4.16108451342339));
#10631=CARTESIAN_POINT('Ctrl Pts',(84.3056684083374,1.68503722575149,-4.09973129194983));
#10632=CARTESIAN_POINT('Ctrl Pts',(84.3132176001518,1.83890268277897,-4.03002407267672));
#10633=CARTESIAN_POINT('Ctrl Pts',(84.3170293094954,1.91659184668235,-3.9948277674892));
#10634=CARTESIAN_POINT('Ctrl Pts',(84.3208417376448,1.9933154911568,-3.95750103751852));
#10635=CARTESIAN_POINT('Ctrl Pts',(84.3246555010349,2.06894820376035,-3.9180881461032));
#10636=CARTESIAN_POINT('Ctrl Pts',(84.3303408196572,2.18169669532784,-3.85933388617491));
#10637=CARTESIAN_POINT('Ctrl Pts',(84.3358434779605,2.29187550637682,-3.79565548959621));
#10638=CARTESIAN_POINT('Ctrl Pts',(84.3410678358074,2.39887081547596,-3.72711308762104));
#10639=CARTESIAN_POINT('Ctrl Pts',(84.346297747787,2.50597987370265,-3.65849781667161));
#10640=CARTESIAN_POINT('Ctrl Pts',(84.3514680195384,2.6100981748788,-3.58533117720361));
#10641=CARTESIAN_POINT('Ctrl Pts',(84.3566430066945,2.71080634011115,-3.50788928878811));
#10642=CARTESIAN_POINT('Ctrl Pts',(84.3618211287584,2.81157551241485,-3.43040048756468));
#10643=CARTESIAN_POINT('Ctrl Pts',(84.3670043347982,2.90893011277071,-3.34863099623333));
#10644=CARTESIAN_POINT('Ctrl Pts',(84.372273141828,3.00246865738971,-3.26289847479069));
#10645=CARTESIAN_POINT('Ctrl Pts',(84.377140630556,3.08888249053952,-3.18369609000235));
#10646=CARTESIAN_POINT('Ctrl Pts',(84.3820816227187,3.1720397850012,-3.10111099545226));
#10647=CARTESIAN_POINT('Ctrl Pts',(84.3871670230929,3.25164114268718,-3.01542965871224));
#10648=CARTESIAN_POINT('Ctrl Pts',(84.3875941892897,3.25832754035971,-3.00823255168778));
#10649=CARTESIAN_POINT('Ctrl Pts',(84.3880223743954,3.26498887791591,-3.00101359155394));
#10650=CARTESIAN_POINT('Ctrl Pts',(84.3884516204334,3.27162499419796,-2.99377294403262));
#10651=CARTESIAN_POINT('Ctrl Pts',(84.3908738698233,3.30907281478261,-2.95291373395086));
#10652=CARTESIAN_POINT('Ctrl Pts',(84.3933299774408,3.34571674374655,-2.91136478436287));
#10653=CARTESIAN_POINT('Ctrl Pts',(84.3958276195801,3.38152702007041,-2.869159449948));
#10654=CARTESIAN_POINT('Ctrl Pts',(84.3958296535773,3.38155618277521,-2.86912507931938));
#10655=CARTESIAN_POINT('Ctrl Pts',(84.395831687602,3.38158534492731,-2.86909070825542));
#10656=CARTESIAN_POINT('Ctrl Pts',(84.3958337216543,3.38161450652671,-2.86905633675616));
#10657=CARTESIAN_POINT('Ctrl Pts',(84.4010193379607,3.4559591379798,-2.78142957766832));
#10658=CARTESIAN_POINT('Ctrl Pts',(84.4063943313847,3.52690871113519,-2.69072693480184));
#10659=CARTESIAN_POINT('Ctrl Pts',(84.4118818220266,3.59423325632701,-2.59726247276966));
#10660=CARTESIAN_POINT('Ctrl Pts',(84.4124385352232,3.60106342064289,-2.58778037925449));
#10661=CARTESIAN_POINT('Ctrl Pts',(84.412996406283,3.6078562742022,-2.57826990430067));
#10662=CARTESIAN_POINT('Ctrl Pts',(84.4135553549299,3.61461157703828,-2.56873140574106));
#10663=CARTESIAN_POINT('Ctrl Pts',(84.4196164272486,3.68786406499651,-2.46529877395051));
#10664=CARTESIAN_POINT('Ctrl Pts',(84.4258036729112,3.75670158311348,-2.35856499542504));
#10665=CARTESIAN_POINT('Ctrl Pts',(84.4320255247527,3.82086467332084,-2.24896710701901));
#10666=CARTESIAN_POINT('Ctrl Pts',(84.4382413353983,3.88496546345941,-2.13947563424797));
#10667=CARTESIAN_POINT('Ctrl Pts',(84.4444913342497,3.9444012366354,-2.02712577217479));
#10668=CARTESIAN_POINT('Ctrl Pts',(84.4507016014946,3.99895415777029,-1.91236493124856));
#10669=CARTESIAN_POINT('Ctrl Pts',(84.4554152926301,4.04036068837952,-1.8252596365421));
#10670=CARTESIAN_POINT('Ctrl Pts',(84.4601059748468,4.07895536305849,-1.73676263301112));
#10671=CARTESIAN_POINT('Ctrl Pts',(84.4646566137891,4.11450449761833,-1.64702193201489));
#10672=CARTESIAN_POINT('Ctrl Pts',(84.4660970909123,4.12575736028934,-1.61861505806947));
#10673=CARTESIAN_POINT('Ctrl Pts',(84.4675235356913,4.13670491876008,-1.59008393111965));
#10674=CARTESIAN_POINT('Ctrl Pts',(84.4689322360632,4.1473394108455,-1.56143427734726));
#10675=CARTESIAN_POINT('Ctrl Pts',(84.4738515811032,4.18447629029761,-1.46138636439162));
#10676=CARTESIAN_POINT('Ctrl Pts',(84.4786476553848,4.21794505108998,-1.35995378726379));
#10677=CARTESIAN_POINT('Ctrl Pts',(84.4834231452708,4.24785814235454,-1.25747763211181));
#10678=CARTESIAN_POINT('Ctrl Pts',(84.4843331475761,4.25355828677076,-1.237950098885));
#10679=CARTESIAN_POINT('Ctrl Pts',(84.4852424024226,4.25912935472623,-1.21838452374533));
#10680=CARTESIAN_POINT('Ctrl Pts',(84.486151620347,4.26457216996989,-1.19878305716253));
#10681=CARTESIAN_POINT('Ctrl Pts',(84.4937000912189,4.30975928213367,-1.03604858439437));
#10682=CARTESIAN_POINT('Ctrl Pts',(84.5012460990225,4.34611122439299,-0.870839143295207));
#10683=CARTESIAN_POINT('Ctrl Pts',(84.5087949932654,4.37341321007671,-0.704147472553858));
#10684=CARTESIAN_POINT('Ctrl Pts',(84.5126064128654,4.38719792079147,-0.61998522566277));
#10685=CARTESIAN_POINT('Ctrl Pts',(84.516418552402,4.39867471587451,-0.535445277101942));
#10686=CARTESIAN_POINT('Ctrl Pts',(84.5202320281092,4.40781088907457,-0.450656510645831));
#10687=CARTESIAN_POINT('Ctrl Pts',(84.5256130576088,4.42070254521122,-0.331014774716957));
#10688=CARTESIAN_POINT('Ctrl Pts',(84.5308328806464,4.42865113939397,-0.210843533130558));
#10689=CARTESIAN_POINT('Ctrl Pts',(84.5358053747255,4.43140167015233,-0.0906023001580588));
#10690=CARTESIAN_POINT('Ctrl Pts',(84.5360862929687,4.43155705983328,-0.0838093396460685));
#10691=CARTESIAN_POINT('Ctrl Pts',(84.5363664218315,4.43169586038957,-0.0770161695411033));
#10692=CARTESIAN_POINT('Ctrl Pts',(84.5366457457854,4.43181802635749,-0.0702228776517116));
#10693=CARTESIAN_POINT('Ctrl Pts',(84.5418748984192,4.43410506434365,0.0569526104701331));
#10694=CARTESIAN_POINT('Ctrl Pts',(84.5470443992794,4.4309466875094,0.184162749014156));
#10695=CARTESIAN_POINT('Ctrl Pts',(84.552218609817,4.42234015442795,0.310905475783738));
#10696=CARTESIAN_POINT('Ctrl Pts',(84.5573959553126,4.41372840680822,0.437724993613409));
#10697=CARTESIAN_POINT('Ctrl Pts',(84.5625783790404,4.39966151476501,0.564076424817015));
#10698=CARTESIAN_POINT('Ctrl Pts',(84.5678464009617,4.38018123020949,0.689449568885464));
#10699=CARTESIAN_POINT('Ctrl Pts',(84.572713127436,4.36218487066706,0.805272321432545));
#10700=CARTESIAN_POINT('Ctrl Pts',(84.5776533538143,4.33956828933044,0.92026065161261));
#10701=CARTESIAN_POINT('Ctrl Pts',(84.582737983543,4.31240388012754,1.03400661169041));
#10702=CARTESIAN_POINT('Ctrl Pts',(84.5831651303285,4.31012186733797,1.04356211991886));
#10703=CARTESIAN_POINT('Ctrl Pts',(84.5835932962048,4.30780777020741,1.05310888891236));
#10704=CARTESIAN_POINT('Ctrl Pts',(84.5840225232079,4.30546163731095,1.06264669262437));
#10705=CARTESIAN_POINT('Ctrl Pts',(84.5864476969319,4.29220576148621,1.11653619813248));
#10706=CARTESIAN_POINT('Ctrl Pts',(84.5889068199102,4.27792749735515,1.17013839040833));
#10707=CARTESIAN_POINT('Ctrl Pts',(84.5914075994229,4.2626381487069,1.22340983725583));
#10708=CARTESIAN_POINT('Ctrl Pts',(84.591409635184,4.26262570240342,1.22345320290926));
#10709=CARTESIAN_POINT('Ctrl Pts',(84.5914116709727,4.26261325542998,1.22349656834367));
#10710=CARTESIAN_POINT('Ctrl Pts',(84.591413706789,4.26260080778662,1.22353993355905));
#10711=CARTESIAN_POINT('Ctrl Pts',(84.5965988639289,4.23089706942438,1.33398971130982));
#10712=CARTESIAN_POINT('Ctrl Pts',(84.6019734473727,4.19475153083039,1.44331960372824));
#10713=CARTESIAN_POINT('Ctrl Pts',(84.607460578133,4.15429803545426,1.55116413066714));
#10714=CARTESIAN_POINT('Ctrl Pts',(84.6080174542468,4.15019250448003,1.56210902038882));
#10715=CARTESIAN_POINT('Ctrl Pts',(84.6085754895695,4.14604263913158,1.57303858616504));
#10716=CARTESIAN_POINT('Ctrl Pts',(84.6091346037398,4.14184860431232,1.58395242950338));
#10717=CARTESIAN_POINT('Ctrl Pts',(84.6151954975086,4.09638454552827,1.70226036839237));
#10718=CARTESIAN_POINT('Ctrl Pts',(84.6213826301699,4.04572545282814,1.81872446903964));
#10719=CARTESIAN_POINT('Ctrl Pts',(84.6276044230074,3.99009117374434,1.93288649496196));
#10720=CARTESIAN_POINT('Ctrl Pts',(84.6338201725864,3.93451093251407,2.04693763473753));
#10721=CARTESIAN_POINT('Ctrl Pts',(84.6400701641749,3.87396548678901,2.1586913614496));
#10722=CARTESIAN_POINT('Ctrl Pts',(84.6462804649277,3.80870639577885,2.26771832871206));
#10723=CARTESIAN_POINT('Ctrl Pts',(84.65100029518,3.75910946895452,2.35057885333004));
#10724=CARTESIAN_POINT('Ctrl Pts',(84.6556970803124,3.70678832164182,2.43186689386273));
#10725=CARTESIAN_POINT('Ctrl Pts',(84.660253925992,3.65173737784779,2.51130545350703));
#10726=CARTESIAN_POINT('Ctrl Pts',(84.6616885949146,3.63440523983481,2.53631574369312));
#10727=CARTESIAN_POINT('Ctrl Pts',(84.6631093926092,3.61680274000409,2.56114239081144));
#10728=CARTESIAN_POINT('Ctrl Pts',(84.6645126710695,3.59893035714528,2.58577590195689));
#10729=CARTESIAN_POINT('Ctrl Pts',(84.6694225893463,3.53639683886947,2.67196587066897));
#10730=CARTESIAN_POINT('Ctrl Pts',(84.674208683927,3.47068942515095,2.75587981751586));
#10731=CARTESIAN_POINT('Ctrl Pts',(84.6789738848567,3.4021535104872,2.83742357267385));
#10732=CARTESIAN_POINT('Ctrl Pts',(84.679894240563,3.38891641490988,2.85317301566378));
#10733=CARTESIAN_POINT('Ctrl Pts',(84.6808138168642,3.37557370148446,2.8688341578141));
#10734=CARTESIAN_POINT('Ctrl Pts',(84.6817333553531,3.362127703261,2.88440648181033));
#10735=CARTESIAN_POINT('Ctrl Pts',(84.6892818648234,3.25174924041889,3.01223999457874));
#10736=CARTESIAN_POINT('Ctrl Pts',(84.6968279079958,3.13441231669963,3.13409281579267));
#10737=CARTESIAN_POINT('Ctrl Pts',(84.7043768347802,3.01082409715453,3.24923579076595));
#10738=CARTESIAN_POINT('Ctrl Pts',(84.7081880418649,2.94842843332505,3.30736772587436));
#10739=CARTESIAN_POINT('Ctrl Pts',(84.7119999681048,2.88443900415451,3.36378856116201));
#10740=CARTESIAN_POINT('Ctrl Pts',(84.7158132297576,2.81894492700688,3.41839963964567));
#10741=CARTESIAN_POINT('Ctrl Pts',(84.7212084245133,2.72628060608488,3.49566614560924));
#10742=CARTESIAN_POINT('Ctrl Pts',(84.7264411225267,2.63041772563086,3.56909176912647));
#10743=CARTESIAN_POINT('Ctrl Pts',(84.7314255010948,2.53160030781325,3.63820716678816));
#10744=CARTESIAN_POINT('Ctrl Pts',(84.7316931778632,2.52629350242069,3.64191888050341));
#10745=CARTESIAN_POINT('Ctrl Pts',(84.7319601384716,2.5209781870118,3.64561815736127));
#10746=CARTESIAN_POINT('Ctrl Pts',(84.7322263696277,2.51565440316096,3.64930492268869));
#10747=CARTESIAN_POINT('Ctrl Pts',(84.7374556145453,2.41108598956213,3.7217194331949));
#10748=CARTESIAN_POINT('Ctrl Pts',(84.7426251826069,2.30346961961977,3.78962151737821));
#10749=CARTESIAN_POINT('Ctrl Pts',(84.7477994256095,2.19322158624946,3.85273053620533));
#10750=CARTESIAN_POINT('Ctrl Pts',(84.7529768027908,2.08290677266984,3.9158777818684));
#10751=CARTESIAN_POINT('Ctrl Pts',(84.7581592233412,1.96995698362092,3.97422577405039));
#10752=CARTESIAN_POINT('Ctrl Pts',(84.7634272006878,1.85481995124432,4.02752638811055));
#10753=CARTESIAN_POINT('Ctrl Pts',(84.7682940795581,1.74844933626545,4.07676874723082));
#10754=CARTESIAN_POINT('Ctrl Pts',(84.7732344287618,1.64021136687734,4.12170321913324));
#10755=CARTESIAN_POINT('Ctrl Pts',(84.7783191586336,1.53048571385177,4.16216385123994));
#10756=CARTESIAN_POINT('Ctrl Pts',(84.778746094102,1.52127268302028,4.16556109737866));
#10757=CARTESIAN_POINT('Ctrl Pts',(84.7791740474533,1.51204914634207,4.16892682775203));
#10758=CARTESIAN_POINT('Ctrl Pts',(84.7796030606624,1.50281531855477,4.17226095757485));
#10759=CARTESIAN_POINT('Ctrl Pts',(84.7820291275204,1.45059808353492,4.1911154396548));
#10760=CARTESIAN_POINT('Ctrl Pts',(84.7844891619393,1.39805284444655,4.20895901044887));
#10761=CARTESIAN_POINT('Ctrl Pts',(84.7869908804251,1.3452220621743,4.22577697960224));
#10762=CARTESIAN_POINT('Ctrl Pts',(84.7869929158898,1.34517907764301,4.22579066314979));
#10763=CARTESIAN_POINT('Ctrl Pts',(84.7869949513822,1.3451360929226,4.22580434601856));
#10764=CARTESIAN_POINT('Ctrl Pts',(84.7869969869022,1.34509310801311,4.22581802820855));
#10765=CARTESIAN_POINT('Ctrl Pts',(84.7921822518366,1.23559374319761,4.26067191370071));
#10766=CARTESIAN_POINT('Ctrl Pts',(84.7975569329699,1.12456366365035,4.29120810213901));
#10767=CARTESIAN_POINT('Ctrl Pts',(84.8030441534666,1.01238125775074,4.31733535217763));
#10768=CARTESIAN_POINT('Ctrl Pts',(84.8036010288402,1.00099632812464,4.31998689901002));
#10769=CARTESIAN_POINT('Ctrl Pts',(84.8041590632998,0.9895995713314,4.32259305297463));
#10770=CARTESIAN_POINT('Ctrl Pts',(84.8047181764906,0.978191410431902,4.32515373038107));
#10771=CARTESIAN_POINT('Ctrl Pts',(84.8107791588467,0.854522959968089,4.35291236823539));
#10772=CARTESIAN_POINT('Ctrl Pts',(84.81696637055,0.729508691004713,4.37532504084231));
#10773=CARTESIAN_POINT('Ctrl Pts',(84.8231882360403,0.603651872050102,4.39232065761651));
#10774=CARTESIAN_POINT('Ctrl Pts',(84.8294040599685,0.477917262707511,4.40929977129021));
#10775=CARTESIAN_POINT('Ctrl Pts',(84.8356541195363,0.351341757595756,4.42087271830061));
#10776=CARTESIAN_POINT('Ctrl Pts',(84.8418644850906,0.224422162691511,4.42701081737272));
#10777=CARTESIAN_POINT('Ctrl Pts',(84.846584481589,0.127960845190481,4.43167588996372));
#10778=CARTESIAN_POINT('Ctrl Pts',(84.8512814299853,0.0312977998886688,
4.43320167315009));
#10779=CARTESIAN_POINT('Ctrl Pts',(84.8558384408538,-0.065339516415513,
4.43142996286704));
#10780=CARTESIAN_POINT('Ctrl Pts',(84.8572730147889,-0.0957615143271973,
4.43087221800623));
#10781=CARTESIAN_POINT('Ctrl Pts',(84.858693720529,-0.126180574620701,4.42998769318179));
#10782=CARTESIAN_POINT('Ctrl Pts',(84.8600969113421,-0.15658853336999,4.42877152555789));
#10783=CARTESIAN_POINT('Ctrl Pts',(84.8650070541574,-0.262994175985198,
4.4245158272844));
#10784=CARTESIAN_POINT('Ctrl Pts',(84.8697933831841,-0.369265327470869,
4.41635646912889));
#10785=CARTESIAN_POINT('Ctrl Pts',(84.8745588233476,-0.475132086597381,
4.40452868377238));
#10786=CARTESIAN_POINT('Ctrl Pts',(84.8754790548376,-0.495575513048501,
4.40224467638413));
#10787=CARTESIAN_POINT('Ctrl Pts',(84.8763985073895,-0.516004014129667,
4.39982385132363));
#10788=CARTESIAN_POINT('Ctrl Pts',(84.8773179221476,-0.536415866514308,
4.39726786245597));
#10789=CARTESIAN_POINT('Ctrl Pts',(84.8848664844736,-0.704000885742749,
4.37628272913923));
#10790=CARTESIAN_POINT('Ctrl Pts',(84.8924125810314,-0.870466541977115,
4.34619055125258));
#10791=CARTESIAN_POINT('Ctrl Pts',(84.8999615615935,-1.03481393150272,4.30717557716655));
#10792=CARTESIAN_POINT('Ctrl Pts',(84.903772953535,-1.1177910051455,4.28747737333592));
#10793=CARTESIAN_POINT('Ctrl Pts',(84.9075850647847,-1.20022762712079,4.26550388113197));
#10794=CARTESIAN_POINT('Ctrl Pts',(84.9113985116357,-1.28199226514604,4.24127456962471));
#10795=CARTESIAN_POINT('Ctrl Pts',(84.9170835661561,-1.40388630043182,4.20515371563275));
#10796=CARTESIAN_POINT('Ctrl Pts',(84.9225878106938,-1.52420041891705,4.16371187006001));
#10797=CARTESIAN_POINT('Ctrl Pts',(84.9278116334488,-1.64231834212475,4.11688424728089));
#10798=CARTESIAN_POINT('Ctrl Pts',(84.9330410104032,-1.76056185353242,4.07000683530217));
#10799=CARTESIAN_POINT('Ctrl Pts',(84.9382107268945,-1.87673977245805,4.01809080361348));
#10800=CARTESIAN_POINT('Ctrl Pts',(84.9433851385672,-1.9903877189014,3.96132701634406));
#10801=CARTESIAN_POINT('Ctrl Pts',(84.9485626848299,-2.10410451176347,3.90452884232514));
#10802=CARTESIAN_POINT('Ctrl Pts',(84.9537452947748,-2.21528801804004,3.84287672460635));
#10803=CARTESIAN_POINT('Ctrl Pts',(84.9590134846708,-2.3234834856855,3.77660572067685));
#10804=CARTESIAN_POINT('Ctrl Pts',(84.9638804636316,-2.42343908240562,3.71538173517016));
#10805=CARTESIAN_POINT('Ctrl Pts',(84.968820929834,-2.52084483146928,3.65021526271105));
#10806=CARTESIAN_POINT('Ctrl Pts',(84.9739057901906,-2.61535212615944,3.58133026333488));
#10807=CARTESIAN_POINT('Ctrl Pts',(84.9743328450834,-2.62328937512469,3.57554491743315));
#10808=CARTESIAN_POINT('Ctrl Pts',(84.9747609184714,-2.63120621006221,3.56973334163662));
#10809=CARTESIAN_POINT('Ctrl Pts',(84.9751900523596,-2.63910244121295,3.56389566774748));
#10810=CARTESIAN_POINT('Ctrl Pts',(84.9776149327083,-2.68372118671921,3.53090908457431));
#10811=CARTESIAN_POINT('Ctrl Pts',(84.980073748826,-2.72768115457495,3.49708990838663));
#10812=CARTESIAN_POINT('Ctrl Pts',(84.9825742047632,-2.77094663309581,3.46246528852012));
#10813=CARTESIAN_POINT('Ctrl Pts',(84.9825762399658,-2.7709818482784,3.46243710641392));
#10814=CARTESIAN_POINT('Ctrl Pts',(84.9825782751959,-2.77101706300107,3.46240892377413));
#10815=CARTESIAN_POINT('Ctrl Pts',(84.9825803104536,-2.77105227726383,3.46238074060078));
#10816=CARTESIAN_POINT('Ctrl Pts',(84.9877238771902,-2.86004685909416,3.39115534695546));
#10817=CARTESIAN_POINT('Ctrl Pts',(84.9930545253852,-2.94635632162763,3.31630800407411));
#10818=CARTESIAN_POINT('Ctrl Pts',(84.9984971023633,-3.02969499108077,3.23809704268377));
#10819=CARTESIAN_POINT('Ctrl Pts',(84.9990297304268,-3.03785078094115,3.23044306680363));
#10820=CARTESIAN_POINT('Ctrl Pts',(84.9995634304557,-3.04597811147377,3.22275691735968));
#10821=CARTESIAN_POINT('Ctrl Pts',(85.0000981320124,-3.05407671060235,3.21503886286153));
#10822=CARTESIAN_POINT('Ctrl Pts',(85.0060892369383,-3.14481809056789,3.12856132462402));
#10823=CARTESIAN_POINT('Ctrl Pts',(85.0122055586422,-3.23195384081772,3.03807262820168));
#10824=CARTESIAN_POINT('Ctrl Pts',(85.0183580489291,-3.31514896565735,2.94394188123819));
#10825=CARTESIAN_POINT('Ctrl Pts',(85.0245046105112,-3.39826392144045,2.84990184119039));
#10826=CARTESIAN_POINT('Ctrl Pts',(85.0306869278022,-3.47744610828712,2.75222700492221));
#10827=CARTESIAN_POINT('Ctrl Pts',(85.0368326469943,-3.5523992728702,2.65130570457177));
#10828=CARTESIAN_POINT('Ctrl Pts',(85.0416525936159,-3.61118332093922,2.57215544315203));
#10829=CARTESIAN_POINT('Ctrl Pts',(85.0464499027595,-3.6673678199014,2.4910059570415));
#10830=CARTESIAN_POINT('Ctrl Pts',(85.0511099558291,-3.7206914611155,2.40797628678268));
#10831=CARTESIAN_POINT('Ctrl Pts',(85.0523876421982,-3.73531165717613,2.38521133618301));
#10832=CARTESIAN_POINT('Ctrl Pts',(85.0536550104997,-3.74971663560365,2.36230530365738));
#10833=CARTESIAN_POINT('Ctrl Pts',(85.0549096983235,-3.76390067855733,2.33926124211762));
#10834=CARTESIAN_POINT('Ctrl Pts',(85.0596190440185,-3.81713907009516,2.25276765387323));
#10835=CARTESIAN_POINT('Ctrl Pts',(85.064193515815,-3.86732725704643,2.16437299960269));
#10836=CARTESIAN_POINT('Ctrl Pts',(85.0687410834779,-3.91452920585602,2.0744106404933));
#10837=CARTESIAN_POINT('Ctrl Pts',(85.0698220587615,-3.92574930059326,2.05302622274258));
#10838=CARTESIAN_POINT('Ctrl Pts',(85.070901513875,-3.93680077182231,2.03155301986239));
#10839=CARTESIAN_POINT('Ctrl Pts',(85.071980898965,-3.94768466915442,2.00999512024761));
#10840=CARTESIAN_POINT('Ctrl Pts',(85.079830432555,-4.02683484316675,1.85322117670665));
#10841=CARTESIAN_POINT('Ctrl Pts',(85.0876763508747,-4.09712788891073,1.69196762578581));
#10842=CARTESIAN_POINT('Ctrl Pts',(85.0955238651024,-4.15811534380005,1.52730392757633));
#10843=CARTESIAN_POINT('Ctrl Pts',(85.0989133218668,-4.18445672216733,1.45618325553379));
#10844=CARTESIAN_POINT('Ctrl Pts',(85.102303063988,-4.20906143190783,1.38442637930852));
#10845=CARTESIAN_POINT('Ctrl Pts',(85.1056934694908,-4.23189027752621,1.31211936362746));
#10846=CARTESIAN_POINT('Ctrl Pts',(85.1099652092317,-4.26065347030312,1.22101617488443));
#10847=CARTESIAN_POINT('Ctrl Pts',(85.1141833523306,-4.2865081857872,1.12900683519562));
#10848=CARTESIAN_POINT('Ctrl Pts',(85.1182333576414,-4.30916968856113,1.03625490534938));
#10849=CARTESIAN_POINT('Ctrl Pts',(85.119516655342,-4.31635028517076,1.00686523072654));
#10850=CARTESIAN_POINT('Ctrl Pts',(85.1207830716226,-4.32321018977212,0.977401381275448));
#10851=CARTESIAN_POINT('Ctrl Pts',(85.1220289624946,-4.32974014619538,0.947869635297526));
#10852=CARTESIAN_POINT('Ctrl Pts',(85.1272093075156,-4.35689134218187,0.82507827638232));
#10853=CARTESIAN_POINT('Ctrl Pts',(85.1323260084032,-4.37882950923063,0.701223348312286));
#10854=CARTESIAN_POINT('Ctrl Pts',(85.1374393902874,-4.39546272646208,0.576786473790793));
#10855=CARTESIAN_POINT('Ctrl Pts',(85.1425596171888,-4.41211820971229,0.452183022127615));
#10856=CARTESIAN_POINT('Ctrl Pts',(85.1476768541827,-4.42345416743842,0.32699612501574));
#10857=CARTESIAN_POINT('Ctrl Pts',(85.1528672740182,-4.4294206875847,0.201723058512749));
#10858=CARTESIAN_POINT('Ctrl Pts',(85.1556837299412,-4.43265827559063,0.133746655578993));
#10859=CARTESIAN_POINT('Ctrl Pts',(85.1585219777014,-4.43431563427999,0.0657451159004957));
#10860=CARTESIAN_POINT('Ctrl Pts',(85.1613954767413,-4.43439065261444,-0.002200575292715));
#10861=CARTESIAN_POINT('',(86.4138081402417,-4.43299862504029,0.0034914740243378));
#10862=CARTESIAN_POINT('Ctrl Pts',(85.161395476779,-4.43439065261542,-0.00220057618339957));
#10863=CARTESIAN_POINT('Ctrl Pts',(85.1668210831384,-4.43453229869629,-0.130492449284717));
#10864=CARTESIAN_POINT('Ctrl Pts',(85.1723744448677,-4.42903259483677,-0.258660663528824));
#10865=CARTESIAN_POINT('Ctrl Pts',(85.1781567135762,-4.41786942497314,-0.386319371256166));
#10866=CARTESIAN_POINT('Ctrl Pts',(85.1781587489918,-4.41786549542721,-0.386364308380804));
#10867=CARTESIAN_POINT('Ctrl Pts',(85.1781607844358,-4.41786156517934,-0.38640924544292));
#10868=CARTESIAN_POINT('Ctrl Pts',(85.1781628199082,-4.41785763422956,-0.386454182442532));
#10869=CARTESIAN_POINT('Ctrl Pts',(85.1833480825578,-4.40784373897282,-0.50092891047146));
#10870=CARTESIAN_POINT('Ctrl Pts',(85.1887227609473,-4.3932557495046,-0.615153120549821));
#10871=CARTESIAN_POINT('Ctrl Pts',(85.1942099770911,-4.37415521245614,-0.72874247943483));
#10872=CARTESIAN_POINT('Ctrl Pts',(85.1947668349711,-4.37221683709614,-0.740269841930538));
#10873=CARTESIAN_POINT('Ctrl Pts',(85.1953248518495,-4.37023201915508,-0.751790634686316));
#10874=CARTESIAN_POINT('Ctrl Pts',(85.1958839473777,-4.36820084434691,-0.763304435090718));
#10875=CARTESIAN_POINT('Ctrl Pts',(85.2019449060681,-4.34618159006043,-0.888121510356143));
#10876=CARTESIAN_POINT('Ctrl Pts',(85.2081320915797,-4.31871057529508,-1.0121213732573));
#10877=CARTESIAN_POINT('Ctrl Pts',(85.2143539280782,-4.285916042659,-1.1348122127836));
#10878=CARTESIAN_POINT('Ctrl Pts',(85.2205697224126,-4.25315335752385,-1.25738390450353));
#10879=CARTESIAN_POINT('Ctrl Pts',(85.2268197495983,-4.2150778415336,-1.3786492408531));
#10880=CARTESIAN_POINT('Ctrl Pts',(85.2330300798527,-4.17185438485228,-1.49813870943444));
#10881=CARTESIAN_POINT('Ctrl Pts',(85.2377493203303,-4.13900880692024,-1.5889389589675));
#10882=CARTESIAN_POINT('Ctrl Pts',(85.2424455181467,-4.10318943663691,-1.67871648935425));
#10883=CARTESIAN_POINT('Ctrl Pts',(85.247001766108,-4.06433780339744,-1.76720053099714));
#10884=CARTESIAN_POINT('Ctrl Pts',(85.2484370249745,-4.05209919137351,-1.79507379566279));
#10885=CARTESIAN_POINT('Ctrl Pts',(85.2498583965279,-4.03955984543033,-1.82281835246469));
#10886=CARTESIAN_POINT('Ctrl Pts',(85.2512622264202,-4.02671841734579,-1.85042477828402));
#10887=CARTESIAN_POINT('Ctrl Pts',(85.2561732876982,-3.98179485462209,-1.94700118658597));
#10888=CARTESIAN_POINT('Ctrl Pts',(85.2609605908363,-3.93331931290938,-2.04194920990385));
#10889=CARTESIAN_POINT('Ctrl Pts',(85.2657270366361,-3.8816128907154,-2.13511023544705));
#10890=CARTESIAN_POINT('Ctrl Pts',(85.2666461992026,-3.87164181169204,-2.15307543025598));
#10891=CARTESIAN_POINT('Ctrl Pts',(85.2675645861398,-3.86155050396846,-2.17097430434491));
#10892=CARTESIAN_POINT('Ctrl Pts',(85.2684829353718,-3.85134114898564,-2.18880590722276));
#10893=CARTESIAN_POINT('Ctrl Pts',(85.2760314676801,-3.7674235681314,-2.33537588924219));
#10894=CARTESIAN_POINT('Ctrl Pts',(85.2835775343156,-3.67553289452415,-2.47740499943486));
#10895=CARTESIAN_POINT('Ctrl Pts',(85.2911264850738,-3.57622392108629,-2.6140423864284));
#10896=CARTESIAN_POINT('Ctrl Pts',(85.2949378100764,-3.5260846652396,-2.68302806483719));
#10897=CARTESIAN_POINT('Ctrl Pts',(85.2987498543982,-3.47405393029844,-2.75063862976931));
#10898=CARTESIAN_POINT('Ctrl Pts',(85.3025632343123,-3.42020034436607,-2.81676020277861));
#10899=CARTESIAN_POINT('Ctrl Pts',(85.3079619474277,-3.34395825277632,-2.91037044131991));
#10900=CARTESIAN_POINT('Ctrl Pts',(85.3131978229635,-3.26383738623406,-3.00081748735583));
#10901=CARTESIAN_POINT('Ctrl Pts',(85.3181851131229,-3.17998820549575,-3.08759329103002));
#10902=CARTESIAN_POINT('Ctrl Pts',(85.3184495881628,-3.17554169953457,-3.09219499524378));
#10903=CARTESIAN_POINT('Ctrl Pts',(85.3187133641408,-3.17108471831213,-3.09678636750796));
#10904=CARTESIAN_POINT('Ctrl Pts',(85.3189764282693,-3.16661728747347,-3.10136732949371));
#10905=CARTESIAN_POINT('Ctrl Pts',(85.3242057306658,-3.07781176723478,-3.19242967092221));
#10906=CARTESIAN_POINT('Ctrl Pts',(85.3293753673474,-2.98515211965728,-3.27964505079976));
#10907=CARTESIAN_POINT('Ctrl Pts',(85.3345496931392,-2.88899334977489,-3.36265844604907));
#10908=CARTESIAN_POINT('Ctrl Pts',(85.3397271534056,-2.79277632936137,-3.4457221286967));
#10909=CARTESIAN_POINT('Ctrl Pts',(85.3449096712612,-2.69305575273366,-3.52457838493965));
#10910=CARTESIAN_POINT('Ctrl Pts',(85.3501777623043,-2.5902236990862,-3.5988980996034));
#10911=CARTESIAN_POINT('Ctrl Pts',(85.355044675709,-2.4952225504281,-3.66755819157436));
#10912=CARTESIAN_POINT('Ctrl Pts',(85.3599850713443,-2.3975653103509,-3.73234661030828));
#10913=CARTESIAN_POINT('Ctrl Pts',(85.365069857038,-2.29759293697757,-3.79302791604585));
#10914=CARTESIAN_POINT('Ctrl Pts',(85.3654968768067,-2.28919726755768,-3.79812392573082));
#10915=CARTESIAN_POINT('Ctrl Pts',(85.365924914904,-2.2807852577451,-3.80319099720603));
#10916=CARTESIAN_POINT('Ctrl Pts',(85.3663540133271,-2.27235710222539,-3.80822900614889));
#10917=CARTESIAN_POINT('Ctrl Pts',(85.368779374882,-2.22471925674633,-3.83670497470224));
#10918=CARTESIAN_POINT('Ctrl Pts',(85.3712386857147,-2.17656659910718,-3.86425190211056));
#10919=CARTESIAN_POINT('Ctrl Pts',(85.373739654942,-2.12793796450106,-3.89084727575266));
#10920=CARTESIAN_POINT('Ctrl Pts',(85.373741690305,-2.12789838907449,-3.89086891985731));
#10921=CARTESIAN_POINT('Ctrl Pts',(85.3737437256956,-2.12785881333261,-3.8908905633319));
#10922=CARTESIAN_POINT('Ctrl Pts',(85.3737457611138,-2.12781923727546,-3.89091220617643));
#10923=CARTESIAN_POINT('Ctrl Pts',(85.3789310406537,-2.02699822663038,-3.94604790223953));
#10924=CARTESIAN_POINT('Ctrl Pts',(85.384305734269,-1.92384963727594,-3.99723800442516));
#10925=CARTESIAN_POINT('Ctrl Pts',(85.3897929641781,-1.81872744698372,-4.04432064396025));
#10926=CARTESIAN_POINT('Ctrl Pts',(85.3903498198305,-1.80805942562741,-4.04909868942026));
#10927=CARTESIAN_POINT('Ctrl Pts',(85.3909078344512,-1.79737112238041,-4.05383444201256));
#10928=CARTESIAN_POINT('Ctrl Pts',(85.3914669276933,-1.78666293646813,-4.0585277387613));
#10929=CARTESIAN_POINT('Ctrl Pts',(85.397527897637,-1.67057855540134,-4.10940642658978));
#10930=CARTESIAN_POINT('Ctrl Pts',(85.4037150925775,-1.55215160366985,-4.15529490839237));
#10931=CARTESIAN_POINT('Ctrl Pts',(85.4099369371497,-1.43186248333389,-4.19602723197587));
#10932=CARTESIAN_POINT('Ctrl Pts',(85.4161527397556,-1.31169017446999,-4.23672000083767));
#10933=CARTESIAN_POINT('Ctrl Pts',(85.4224027738622,-1.18965940180539,-4.27226698442839));
#10934=CARTESIAN_POINT('Ctrl Pts',(85.4286131101797,-1.06625232866992,-4.30254509279423));
#10935=CARTESIAN_POINT('Ctrl Pts',(85.4333322860001,-0.972476461172645,
-4.32555314092343));
#10936=CARTESIAN_POINT('Ctrl Pts',(85.4380284193404,-0.877902961242614,
-4.3455193671393));
#10937=CARTESIAN_POINT('Ctrl Pts',(85.4425846016461,-0.782724742264051,
-4.36224498294978));
#10938=CARTESIAN_POINT('Ctrl Pts',(85.4440199279464,-0.752740911120412,
-4.36751402502282));
#10939=CARTESIAN_POINT('Ctrl Pts',(85.4454413651113,-0.722697449141261,
-4.37246139612236));
#10940=CARTESIAN_POINT('Ctrl Pts',(85.4468452580771,-0.692601452000684,
-4.37708074842749));
#10941=CARTESIAN_POINT('Ctrl Pts',(85.45175646596,-0.587317287181475,-4.39324052699138));
#10942=CARTESIAN_POINT('Ctrl Pts',(85.4565439239927,-0.481418915382423,
-4.40554118962475));
#10943=CARTESIAN_POINT('Ctrl Pts',(85.461310529251,-0.375216390901607,-4.41416201521859));
#10944=CARTESIAN_POINT('Ctrl Pts',(85.462229543046,-0.35474027010403,-4.41582413264091));
#10945=CARTESIAN_POINT('Ctrl Pts',(85.4631477816843,-0.334252687663094,
-4.41734946659411));
#10946=CARTESIAN_POINT('Ctrl Pts',(85.4640659826311,-0.313755643078922,
-4.418739304735));
#10947=CARTESIAN_POINT('Ctrl Pts',(85.4716145197362,-0.145249280577096,
-4.43016517487088));
#10948=CARTESIAN_POINT('Ctrl Pts',(85.4791605912643,0.0238986476900566,
-4.43243799545198));
#10949=CARTESIAN_POINT('Ctrl Pts',(85.486709546992,0.19267244386593,-4.42554773183715));
#10950=CARTESIAN_POINT('Ctrl Pts',(85.4905208933619,0.27788361990026,-4.42206894852415));
#10951=CARTESIAN_POINT('Ctrl Pts',(85.4943329590767,0.362999100930133,-4.4162535873237));
#10952=CARTESIAN_POINT('Ctrl Pts',(85.4981463604128,0.447886062404757,-4.40809562328451));
#10953=CARTESIAN_POINT('Ctrl Pts',(85.503545883319,0.56808035944329,-4.39654448827011));
#10954=CARTESIAN_POINT('Ctrl Pts',(85.5087824908673,0.687792560931075,-4.38000999976921));
#10955=CARTESIAN_POINT('Ctrl Pts',(85.5137704524758,0.806516216060299,-4.35833571842177));
#10956=CARTESIAN_POINT('Ctrl Pts',(85.5140341877449,0.812793653135961,-4.3571897047047));
#10957=CARTESIAN_POINT('Ctrl Pts',(85.514297227875,0.819068314902127,-4.35602932510892));
#10958=CARTESIAN_POINT('Ctrl Pts',(85.5145595601936,0.825340122617658,-4.35485455774603));
#10959=CARTESIAN_POINT('Ctrl Pts',(85.5197888746267,0.950361907167116,-4.33143682576176));
#10960=CARTESIAN_POINT('Ctrl Pts',(85.5249585253223,1.07431902705324,-4.30267866714438));
#10961=CARTESIAN_POINT('Ctrl Pts',(85.5301328676191,1.1967191926631,-4.26867868766901));
#10962=CARTESIAN_POINT('Ctrl Pts',(85.5353103444421,1.31919350615623,-4.2346581115997));
#10963=CARTESIAN_POINT('Ctrl Pts',(85.5404928813545,1.44010879488779,-4.19538900741506));
#10964=CARTESIAN_POINT('Ctrl Pts',(85.5457609943259,1.55897377497918,-4.1510151994597));
#10965=CARTESIAN_POINT('Ctrl Pts',(85.5506279157658,1.66878662887889,-4.11002066527285));
#10966=CARTESIAN_POINT('Ctrl Pts',(85.5555683215245,1.77685002086513,-4.06466906424268));
#10967=CARTESIAN_POINT('Ctrl Pts',(85.5606531189954,1.88277897280011,-4.01511361269659));
#10968=CARTESIAN_POINT('Ctrl Pts',(85.5610801535461,1.89167516240454,-4.01095181665468));
#10969=CARTESIAN_POINT('Ctrl Pts',(85.5615082065029,1.90055632770093,-4.00676037537719));
#10970=CARTESIAN_POINT('Ctrl Pts',(85.5619373198668,1.90942225726392,-4.00253938196578));
#10971=CARTESIAN_POINT('Ctrl Pts',(85.5643625504949,1.95953005099265,-3.97868348894449));
#10972=CARTESIAN_POINT('Ctrl Pts',(85.5668217269671,2.00915016073338,-3.95388416756324));
#10973=CARTESIAN_POINT('Ctrl Pts',(85.5693225570282,2.05824232611497,-3.92816125207459));
#10974=CARTESIAN_POINT('Ctrl Pts',(85.5693245923688,2.05828228056004,-3.92814031706783));
#10975=CARTESIAN_POINT('Ctrl Pts',(85.569326627737,2.05832223465556,-3.92811938144936));
#10976=CARTESIAN_POINT('Ctrl Pts',(85.5693286631328,2.05836218840156,-3.92809844521918));
#10977=CARTESIAN_POINT('Ctrl Pts',(85.5745139464288,2.1601465653664,-3.87476224128411));
#10978=CARTESIAN_POINT('Ctrl Pts',(85.5798886432999,2.25993783174311,-3.81730137882095));
#10979=CARTESIAN_POINT('Ctrl Pts',(85.5853758757969,2.35740501692618,-3.75592069956012));
#10980=CARTESIAN_POINT('Ctrl Pts',(85.585932727575,2.36729611875289,-3.7496917051799));
#10981=CARTESIAN_POINT('Ctrl Pts',(85.5864907382973,2.37716326893364,-3.74342238349453));
#10982=CARTESIAN_POINT('Ctrl Pts',(85.5870498276185,2.38700611049728,-3.73711297638262));
#10983=CARTESIAN_POINT('Ctrl Pts',(85.5931107958598,2.49371025929989,-3.66871403782689));
#10984=CARTESIAN_POINT('Ctrl Pts',(85.5992979881655,2.59756026347723,-3.59559879567256));
#10985=CARTESIAN_POINT('Ctrl Pts',(85.6055198292351,2.69815166011257,-3.51807504018558));
#10986=CARTESIAN_POINT('Ctrl Pts',(85.6117356282732,2.79864537241397,-3.44062656803964));
#10987=CARTESIAN_POINT('Ctrl Pts',(85.6179856579474,2.89588705574694,-3.35877841704357));
#10988=CARTESIAN_POINT('Ctrl Pts',(85.6241959890656,2.98950694150772,-3.27286360781744));
#10989=CARTESIAN_POINT('Ctrl Pts',(85.6289150054429,3.06064546306844,-3.20757990811144));
#10990=CARTESIAN_POINT('Ctrl Pts',(85.6336109804167,3.12969489087132,-3.13994605065859));
#10991=CARTESIAN_POINT('Ctrl Pts',(85.6381670017238,3.19638283688527,-3.0700123430786));
#10992=CARTESIAN_POINT('Ctrl Pts',(85.639602474662,3.21739431496035,-3.0479782177028));
#10993=CARTESIAN_POINT('Ctrl Pts',(85.6410240543836,3.23817110296885,-3.02571606961333));
#10994=CARTESIAN_POINT('Ctrl Pts',(85.6424280842009,3.25870398038264,-3.00322828479843));
#10995=CARTESIAN_POINT('Ctrl Pts',(85.6473395029352,3.33052977606849,-2.92456405255317));
#10996=CARTESIAN_POINT('Ctrl Pts',(85.6521271844414,3.39948421486727,-2.8432487856963));
#10997=CARTESIAN_POINT('Ctrl Pts',(85.6568940202897,3.4655445640575,-2.75963994234371));
#10998=CARTESIAN_POINT('Ctrl Pts',(85.6578127941348,3.47827722844288,-2.74352493000865));
#10999=CARTESIAN_POINT('Ctrl Pts',(85.6587307935673,3.49090246941608,-2.72732458602232));
#11000=CARTESIAN_POINT('Ctrl Pts',(85.6596487553285,3.50342024982663,-2.71104128631642));
#11001=CARTESIAN_POINT('Ctrl Pts',(85.6671972879246,3.60635577225999,-2.57714135300609));
#11002=CARTESIAN_POINT('Ctrl Pts',(85.6747433549857,3.70202963259365,-2.43763268107927));
#11003=CARTESIAN_POINT('Ctrl Pts',(85.6822923062878,3.78987033601152,-2.29335499308759));
#11004=CARTESIAN_POINT('Ctrl Pts',(85.6861036452507,3.83421963461832,-2.22051160707096));
#11005=CARTESIAN_POINT('Ctrl Pts',(85.689915703567,3.876571329252,-2.14645237246497));
#11006=CARTESIAN_POINT('Ctrl Pts',(85.6937290975101,3.91684676285031,-2.07128448789889));
#11007=CARTESIAN_POINT('Ctrl Pts',(85.6991276026451,3.97386346197388,-1.96487161347015));
#11008=CARTESIAN_POINT('Ctrl Pts',(85.7043632878672,4.0264673221173,-1.85609789432114));
#11009=CARTESIAN_POINT('Ctrl Pts',(85.709350401024,4.07424747782251,-1.74529782869364));
#11010=CARTESIAN_POINT('Ctrl Pts',(85.7096150758851,4.07678325466876,-1.73941747445799));
#11011=CARTESIAN_POINT('Ctrl Pts',(85.7098790506152,4.07930544138933,-1.73353142445952));
#11012=CARTESIAN_POINT('Ctrl Pts',(85.710142312396,4.08181397543319,-1.72763973265671));
#11013=CARTESIAN_POINT('Ctrl Pts',(85.7153716156603,4.13164226887822,-1.61061004802642));
#11014=CARTESIAN_POINT('Ctrl Pts',(85.720541254681,4.17643585074539,-1.49150545855224));
#11015=CARTESIAN_POINT('Ctrl Pts',(85.7257155847687,4.21600383827358,-1.37079032936255));
#11016=CARTESIAN_POINT('Ctrl Pts',(85.7308930493736,4.2555957953849,-1.25000207309453));
#11017=CARTESIAN_POINT('Ctrl Pts',(85.7360755735318,4.28995542827685,-1.12760128145018));
#11018=CARTESIAN_POINT('Ctrl Pts',(85.7413436731781,4.31893004376428,-1.00407655350216));
#11019=CARTESIAN_POINT('Ctrl Pts',(85.7462105841652,4.34569811649109,-0.889958769861308));
#11020=CARTESIAN_POINT('Ctrl Pts',(85.7511509790384,4.36787016929533,-0.774881197198832));
#11021=CARTESIAN_POINT('Ctrl Pts',(85.7562357652567,4.38536026521319,-0.659249172339784));
#11022=CARTESIAN_POINT('Ctrl Pts',(85.7566627968089,4.38682912201197,-0.649538140069354));
#11023=CARTESIAN_POINT('Ctrl Pts',(85.7570908467547,4.3882649776261,-0.639823174911116));
#11024=CARTESIAN_POINT('Ctrl Pts',(85.7575199570946,4.38966779231492,-0.630104504434078));
#11025=CARTESIAN_POINT('Ctrl Pts',(85.7599452465974,4.39759636317974,-0.575175533271245));
#11026=CARTESIAN_POINT('Ctrl Pts',(85.7624044836573,4.40446934448957,-0.520129343393918));
#11027=CARTESIAN_POINT('Ctrl Pts',(85.7649053766406,4.41028092039038,-0.465010440849745));
#11028=CARTESIAN_POINT('Ctrl Pts',(85.7649074120062,4.41028565017342,-0.464965582027521));
#11029=CARTESIAN_POINT('Ctrl Pts',(85.7649094473993,4.41029037925355,-0.464920723157004));
#11030=CARTESIAN_POINT('Ctrl Pts',(85.76491148282,4.4102951076308,-0.464875864238241));
#11031=CARTESIAN_POINT('Ctrl Pts',(85.7700967600214,4.42234074844375,-0.350596822083761));
#11032=CARTESIAN_POINT('Ctrl Pts',(85.7754714514693,4.42984869433835,-0.23568961969063));
#11033=CARTESIAN_POINT('Ctrl Pts',(85.7809586792566,4.43280591622131,-0.120543270618313));
#11034=CARTESIAN_POINT('Ctrl Pts',(85.781515533675,4.43310602077966,-0.108857997885254));
#11035=CARTESIAN_POINT('Ctrl Pts',(85.7820735470579,4.43335928376502,-0.097170299192586));
#11036=CARTESIAN_POINT('Ctrl Pts',(85.7826326390588,4.43356570855561,-0.0854806057341502));
#11037=CARTESIAN_POINT('Ctrl Pts',(85.7886936055249,4.43580350435964,0.0412442265748516));
#11038=CARTESIAN_POINT('Ctrl Pts',(85.7948807970002,4.43253382778728,0.168208678150159));
#11039=CARTESIAN_POINT('Ctrl Pts',(85.8011026380361,4.42378857895326,0.294905493997303));
#11040=CARTESIAN_POINT('Ctrl Pts',(85.8073184370284,4.41505182264975,0.421479274285908));
#11041=CARTESIAN_POINT('Ctrl Pts',(85.8135684674508,4.40085049379849,0.547785995504968));
#11042=CARTESIAN_POINT('Ctrl Pts',(85.8197787999398,4.38125672575128,0.673333287428772));
#11043=CARTESIAN_POINT('Ctrl Pts',(85.8244979183678,4.366367778657,0.768734385511546));
#11044=CARTESIAN_POINT('Ctrl Pts',(85.8291939947648,4.34836456394254,0.863699892015333));
#11045=CARTESIAN_POINT('Ctrl Pts',(85.8337501192069,4.32713793572511,0.957975214470737));
#11046=CARTESIAN_POINT('Ctrl Pts',(85.835185496382,4.32045062548277,0.987676037559452));
#11047=CARTESIAN_POINT('Ctrl Pts',(85.8366069829929,4.31344347265241,1.01730798006811));
#11048=CARTESIAN_POINT('Ctrl Pts',(85.8380109234052,4.30611335181733,1.0468620476212));
#11049=CARTESIAN_POINT('Ctrl Pts',(85.8429221924765,4.28047109846406,1.1502481861128));
#11050=CARTESIAN_POINT('Ctrl Pts',(85.8477097154777,4.2510308295093,1.25271461048536));
#11051=CARTESIAN_POINT('Ctrl Pts',(85.8524763878623,4.21807742235806,1.35404423792655));
#11052=CARTESIAN_POINT('Ctrl Pts',(85.8533953276866,4.21172452126983,1.37357900401271));
#11053=CARTESIAN_POINT('Ctrl Pts',(85.854313492581,4.20524099771781,1.39307166603808));
#11054=CARTESIAN_POINT('Ctrl Pts',(85.8552316197899,4.19862880964729,1.41252087509184));
#11055=CARTESIAN_POINT('Ctrl Pts',(85.8627801536881,4.14426561758675,1.57242574711574));
#11056=CARTESIAN_POINT('Ctrl Pts',(85.8703262220055,4.08120854121988,1.72939699634938));
#11057=CARTESIAN_POINT('Ctrl Pts',(85.877875174523,4.0098395593787,1.88249343527474));
#11058=CARTESIAN_POINT('Ctrl Pts',(85.8816865123719,3.97380657319945,1.95978922576486));
#11059=CARTESIAN_POINT('Ctrl Pts',(85.8854985695634,3.93565417893046,2.03609667767147));
#11060=CARTESIAN_POINT('Ctrl Pts',(85.8893119623718,3.89542797929008,2.11129089568053));
#11061=CARTESIAN_POINT('Ctrl Pts',(85.8947108243299,3.83847719822097,2.21774811723718));
#11062=CARTESIAN_POINT('Ctrl Pts',(85.8999468333592,3.77711441206833,2.32184149220192));
#11063=CARTESIAN_POINT('Ctrl Pts',(85.9049342448572,3.71139024578863,2.42304354572274));
#11064=CARTESIAN_POINT('Ctrl Pts',(85.9051985884318,3.70790672311085,2.42840747300297));
#11065=CARTESIAN_POINT('Ctrl Pts',(85.9054622336392,3.70441095599939,2.43376326843933));
#11066=CARTESIAN_POINT('Ctrl Pts',(85.9057251677122,3.70090295464595,2.43911085036852));
#11067=CARTESIAN_POINT('Ctrl Pts',(85.9109544741529,3.63113484182334,2.5454650565884));
#11068=CARTESIAN_POINT('Ctrl Pts',(85.9161241161494,3.55684849920931,2.64877966545965));
#11069=CARTESIAN_POINT('Ctrl Pts',(85.9212984489043,3.47832454955109,2.74863835731252));
#11070=CARTESIAN_POINT('Ctrl Pts',(85.9264759161689,3.39975303161816,2.84855754161014));
#11071=CARTESIAN_POINT('Ctrl Pts',(85.9316584426769,3.31693851450593,2.94501631460888));
#11072=CARTESIAN_POINT('Ctrl Pts',(85.9369265442928,3.23020296281884,3.03761670264264));
#11073=CARTESIAN_POINT('Ctrl Pts',(85.9417934590288,3.15007266818491,3.12316520302148));
#11074=CARTESIAN_POINT('Ctrl Pts',(85.946733857384,3.06659539521238,3.20542092856662));
#11075=CARTESIAN_POINT('Ctrl Pts',(85.9518186468861,2.98006082830787,3.28408762527598));
#11076=CARTESIAN_POINT('Ctrl Pts',(85.9522456765139,2.97279350212243,3.29069419378807));
#11077=CARTESIAN_POINT('Ctrl Pts',(85.9526737245234,2.96550460592939,3.29727547871599));
#11078=CARTESIAN_POINT('Ctrl Pts',(85.9531028329146,2.95819430708086,3.30383132081557));
#11079=CARTESIAN_POINT('Ctrl Pts',(85.9555281218844,2.91687703730188,3.34088445670909));
#11080=CARTESIAN_POINT('Ctrl Pts',(85.9579873583054,2.87487695503373,3.37712409721206));
#11081=CARTESIAN_POINT('Ctrl Pts',(85.960488250536,2.83222787467982,3.41252072634323));
#11082=CARTESIAN_POINT('Ctrl Pts',(85.9604902858933,2.83219316462023,3.41254953397744));
#11083=CARTESIAN_POINT('Ctrl Pts',(85.9604923212782,2.83215845413073,3.41257834105347));
#11084=CARTESIAN_POINT('Ctrl Pts',(85.9604943566907,2.83212374321137,3.41260714757129));
#11085=CARTESIAN_POINT('Ctrl Pts',(85.965679636304,2.74369654677406,3.48599268899348));
#11086=CARTESIAN_POINT('Ctrl Pts',(85.9710543299192,2.65223070046746,3.55595012650461));
#11087=CARTESIAN_POINT('Ctrl Pts',(85.9765415596465,2.55804272712359,3.62225293234593));
#11088=CARTESIAN_POINT('Ctrl Pts',(85.9770984135624,2.54848436262974,3.62898146001987));
#11089=CARTESIAN_POINT('Ctrl Pts',(85.9776564264377,2.53889800842257,3.63567235013124));
#11090=CARTESIAN_POINT('Ctrl Pts',(85.978215517926,2.5292840252238,3.64232536642138));
#11091=CARTESIAN_POINT('Ctrl Pts',(85.9842764857699,2.42506129201463,3.71444901460207));
#11092=CARTESIAN_POINT('Ctrl Pts',(85.9904636783336,2.31758557961003,3.78212206470979));
#11093=CARTESIAN_POINT('Ctrl Pts',(85.9966855202337,2.2072967246636,3.84508982248233));
#11094=CARTESIAN_POINT('Ctrl Pts',(86.0029013201123,2.0971149710608,3.9079964323586));
#11095=CARTESIAN_POINT('Ctrl Pts',(86.0091513511975,1.9841256936657,3.96620722381679));
#11096=CARTESIAN_POINT('Ctrl Pts',(86.0153616841953,1.86877864856529,4.01950923836368));
#11097=CARTESIAN_POINT('Ctrl Pts',(86.0200807854772,1.7811288577099,4.06001231690496));
#11098=CARTESIAN_POINT('Ctrl Pts',(86.0247768448104,1.69211491276211,4.09768213792665));
#11099=CARTESIAN_POINT('Ctrl Pts',(86.0293329518913,1.6018881742771,4.13228671122897));
#11100=CARTESIAN_POINT('Ctrl Pts',(86.0307683458769,1.57346238983785,4.14318882470243));
#11101=CARTESIAN_POINT('Ctrl Pts',(86.0321898488375,1.54491659302445,4.1537865598859));
#11102=CARTESIAN_POINT('Ctrl Pts',(86.0335938049568,1.51625653650733,4.16407232853264));
#11103=CARTESIAN_POINT('Ctrl Pts',(86.038505104712,1.41599832570361,4.2000538612504));
#11104=CARTESIAN_POINT('Ctrl Pts',(86.0432926601702,1.31439973612451,4.23236462215131));
#11105=CARTESIAN_POINT('Ctrl Pts',(86.048059365997,1.21179938123318,4.2611213315272));
#11106=CARTESIAN_POINT('Ctrl Pts',(86.048978273268,1.19202047824482,4.26666493969125));
#11107=CARTESIAN_POINT('Ctrl Pts',(86.0498964057115,1.17220419572373,4.27207650595775));
#11108=CARTESIAN_POINT('Ctrl Pts',(86.0508145004724,1.15235274158155,4.27735691175687));
#11109=CARTESIAN_POINT('Ctrl Pts',(86.0583630347551,0.989134968708486,4.32077217334051));
#11110=CARTESIAN_POINT('Ctrl Pts',(86.0659091034719,0.823538392579329,4.35532565885359));
#11111=CARTESIAN_POINT('Ctrl Pts',(86.0734580564011,0.656558076026867,4.38081342825425));
#11112=CARTESIAN_POINT('Ctrl Pts',(86.0772693966408,0.572252503361662,4.3936817772887));
#11113=CARTESIAN_POINT('Ctrl Pts',(86.081081456227,0.48759436535417,4.40423832719151));
#11114=CARTESIAN_POINT('Ctrl Pts',(86.084894851434,0.402712887044264,4.41245178263173));
#11115=CARTESIAN_POINT('Ctrl Pts',(86.0902937643092,0.282539739172888,4.42408019456336));
#11116=CARTESIAN_POINT('Ctrl Pts',(86.0955298192384,0.161887641220141,4.43072612255225));
#11117=CARTESIAN_POINT('Ctrl Pts',(86.1005172727054,0.0412236526647988,
4.43213924387147));
#11118=CARTESIAN_POINT('Ctrl Pts',(86.1007815702943,0.0348293671928713,
4.43221412869195));
#11119=CARTESIAN_POINT('Ctrl Pts',(86.1010451697595,0.0284350604571021,
4.43227431986939));
#11120=CARTESIAN_POINT('Ctrl Pts',(86.1013080583413,0.0220408060320593,
4.43231978062816));
#11121=CARTESIAN_POINT('Ctrl Pts',(86.1065373657472,-0.10515194534687,4.43322407354545));
#11122=CARTESIAN_POINT('Ctrl Pts',(86.1117070089402,-0.232320156652302,
4.42868291170422));
#11123=CARTESIAN_POINT('Ctrl Pts',(86.1168813431883,-0.358961768078289,
4.41869901193295));
#11124=CARTESIAN_POINT('Ctrl Pts',(86.1220588119524,-0.485680096647177,
4.40870906410009));
#11125=CARTESIAN_POINT('Ctrl Pts',(86.1272413402577,-0.611871074700732,
4.39326939905119));
#11126=CARTESIAN_POINT('Ctrl Pts',(86.1325094440154,-0.737024988835311,
4.37242731107123));
#11127=CARTESIAN_POINT('Ctrl Pts',(86.1373763592312,-0.852647899283205,
4.3531724368732));
#11128=CARTESIAN_POINT('Ctrl Pts',(86.1423167583156,-0.967386181203723,
4.32930648297475));
#11129=CARTESIAN_POINT('Ctrl Pts',(86.1474015487429,-1.08083267256491,4.30090627666888));
#11130=CARTESIAN_POINT('Ctrl Pts',(86.1478285801421,-1.09036014761645,4.29852116758537));
#11131=CARTESIAN_POINT('Ctrl Pts',(86.1482566299326,-1.09987854026065,4.29610408895486));
#11132=CARTESIAN_POINT('Ctrl Pts',(86.1486857401145,-1.10938762518145,4.2936550917611));
#11133=CARTESIAN_POINT('Ctrl Pts',(86.1511110151534,-1.16313173862802,4.27981367756529));
#11134=CARTESIAN_POINT('Ctrl Pts',(86.1535702372874,-1.21657742361984,4.26495298866421));
#11135=CARTESIAN_POINT('Ctrl Pts',(86.156071114729,-1.26968136899565,4.24908480116176));
#11136=CARTESIAN_POINT('Ctrl Pts',(86.1560731500848,-1.26972458799573,4.24907188673155));
#11137=CARTESIAN_POINT('Ctrl Pts',(86.1560751854682,-1.26976780676959,4.24905897163408));
#11138=CARTESIAN_POINT('Ctrl Pts',(86.1560772208791,-1.26981102531726,4.24904605586937));
#11139=CARTESIAN_POINT('Ctrl Pts',(86.1612625006485,-1.37991176874156,4.21614269903718));
#11140=CARTESIAN_POINT('Ctrl Pts',(86.1666371943902,-1.48884431124347,4.17880982876281));
#11141=CARTESIAN_POINT('Ctrl Pts',(86.1721244241947,-1.59624463818395,4.13718526681709));
#11142=CARTESIAN_POINT('Ctrl Pts',(86.1726812777381,-1.60714380857506,4.13296113448877));
#11143=CARTESIAN_POINT('Ctrl Pts',(86.1732392902386,-1.61802717472683,4.12869284075756));
#11144=CARTESIAN_POINT('Ctrl Pts',(86.1737983813502,-1.62889434002148,4.12438055483306));
#11145=CARTESIAN_POINT('Ctrl Pts',(86.1798593488598,-1.74670257271797,4.07763213701908));
#11146=CARTESIAN_POINT('Ctrl Pts',(86.1860465410172,-1.86261049357883,4.02570892503116));
#11147=CARTESIAN_POINT('Ctrl Pts',(86.1922683824398,-1.97616227711835,3.96883574864683));
#11148=CARTESIAN_POINT('Ctrl Pts',(86.1984841818319,-2.089603790515,3.91201780180702));
#11149=CARTESIAN_POINT('Ctrl Pts',(86.2047342123595,-2.2006939357567,3.85025981935736));
#11150=CARTESIAN_POINT('Ctrl Pts',(86.2109445447325,-2.30900612111424,3.78381802623826));
#11151=CARTESIAN_POINT('Ctrl Pts',(86.2156636310042,-2.391310016668,3.73333046213615));
#11152=CARTESIAN_POINT('Ctrl Pts',(86.2203596754306,-2.47201235957494,3.68013676304226));
#11153=CARTESIAN_POINT('Ctrl Pts',(86.2249157673569,-2.5508361628422,3.6242342682063));
#11154=CARTESIAN_POINT('Ctrl Pts',(86.2263511750147,-2.57566979057701,3.60662205351151));
#11155=CARTESIAN_POINT('Ctrl Pts',(86.2277726912659,-2.60031664342907,3.58874119683137));
#11156=CARTESIAN_POINT('Ctrl Pts',(86.2291766601421,-2.62476721643445,3.57059227841078));
#11157=CARTESIAN_POINT('Ctrl Pts',(86.234087978986,-2.71029942585828,3.50710431472075));
#11158=CARTESIAN_POINT('Ctrl Pts',(86.2388755546824,-2.79351987259517,3.44046560918281));
#11159=CARTESIAN_POINT('Ctrl Pts',(86.2436422813972,-2.87433795050354,3.37102268006853));
#11160=CARTESIAN_POINT('Ctrl Pts',(86.2445611666889,-2.88991730873579,3.35763611734187));
#11161=CARTESIAN_POINT('Ctrl Pts',(86.2454792772209,-2.90540750752077,3.34414524224346));
#11162=CARTESIAN_POINT('Ctrl Pts',(86.2463973500722,-2.92080805627222,3.330552380765));
#11163=CARTESIAN_POINT('Ctrl Pts',(86.2539458838062,-3.04743369563578,3.21878981936083));
#11164=CARTESIAN_POINT('Ctrl Pts',(86.2614919519773,-3.168003258343,3.10013424064003));
#11165=CARTESIAN_POINT('Ctrl Pts',(86.2690409043641,-3.28179531821978,2.97530068696945));
#11166=CARTESIAN_POINT('Ctrl Pts',(86.2728522435859,-3.33924701730458,2.91227432318858));
#11167=CARTESIAN_POINT('Ctrl Pts',(86.2766643021547,-3.39497025934898,2.84767279345664));
#11168=CARTESIAN_POINT('Ctrl Pts',(86.2804776963446,-3.44886735218826,2.78158629048153));
#11169=CARTESIAN_POINT('Ctrl Pts',(86.285876501233,-3.52517204921117,2.68802446142602));
#11170=CARTESIAN_POINT('Ctrl Pts',(86.2911124583068,-3.5975959138434,2.59130168136755));
#11171=CARTESIAN_POINT('Ctrl Pts',(86.296099821761,-3.66567168304665,2.49166783635782));
#11172=CARTESIAN_POINT('Ctrl Pts',(86.2963642188998,-3.66928061164577,2.48638590657717));
#11173=CARTESIAN_POINT('Ctrl Pts',(86.2966279173858,-3.67287731448961,2.48109580621379));
#11174=CARTESIAN_POINT('Ctrl Pts',(86.2968909044437,-3.67646172009797,2.47579757615328));
#11175=CARTESIAN_POINT('Ctrl Pts',(86.3021202105473,-3.74773501497731,2.37044613027905));
#11176=CARTESIAN_POINT('Ctrl Pts',(86.3072898523626,-3.81446286795207,2.2620959309462));
#11177=CARTESIAN_POINT('Ctrl Pts',(86.3124641851487,-3.87636917814906,2.15116631049352));
#11178=CARTESIAN_POINT('Ctrl Pts',(86.3176416524492,-3.93831299003523,2.04016949094377));
#11179=CARTESIAN_POINT('Ctrl Pts',(86.3228241792064,-3.995429034636,1.92659000537864));
#11180=CARTESIAN_POINT('Ctrl Pts',(86.3280922813235,-4.04747406603953,1.81087827115258));
#11181=CARTESIAN_POINT('Ctrl Pts',(86.3329591953664,-4.09555564998932,1.70397847086176));
#11182=CARTESIAN_POINT('Ctrl Pts',(86.3378995932091,-4.13930931086627,1.59525831342402));
#11183=CARTESIAN_POINT('Ctrl Pts',(86.3429843823386,-4.17857323934634,1.4850992448709));
#11184=CARTESIAN_POINT('Ctrl Pts',(86.3434114132466,-4.18187070372523,1.47584786278491));
#11185=CARTESIAN_POINT('Ctrl Pts',(86.3438394625435,-4.18513652669808,1.4665863141237));
#11186=CARTESIAN_POINT('Ctrl Pts',(86.3442685722297,-4.18837062577084,1.45731481466741));
#11187=CARTESIAN_POINT('Ctrl Pts',(86.3466938550415,-4.20664941356103,1.40491327493541));
#11188=CARTESIAN_POINT('Ctrl Pts',(86.3491530851702,-4.22391446915204,1.35219496580757));
#11189=CARTESIAN_POINT('Ctrl Pts',(86.35165397091,-4.24015157932302,1.29920246144712));
#11190=CARTESIAN_POINT('Ctrl Pts',(86.3516560062688,-4.24016479397886,1.29915933322416));
#11191=CARTESIAN_POINT('Ctrl Pts',(86.3516580416552,-4.24017800795399,1.29911620481949));
#11192=CARTESIAN_POINT('Ctrl Pts',(86.3516600770691,-4.24019122124841,1.29907307623315));
#11193=CARTESIAN_POINT('Ctrl Pts',(86.3571928480507,-4.27610830445762,1.18183864739698));
#11194=CARTESIAN_POINT('Ctrl Pts',(86.3629366538387,-4.30705822960612,1.06303512474668));
#11195=CARTESIAN_POINT('Ctrl Pts',(86.368801100108,-4.33297671141248,0.943052260128244));
#11196=CARTESIAN_POINT('Ctrl Pts',(86.370235611573,-4.33931667218611,0.913703062097574));
#11197=CARTESIAN_POINT('Ctrl Pts',(86.3716773415401,-4.34535556605231,0.884283542759871));
#11198=CARTESIAN_POINT('Ctrl Pts',(86.3731249669716,-4.35109244908456,0.854799881287111));
#11199=CARTESIAN_POINT('Ctrl Pts',(86.3792815320168,-4.3754906758473,0.729409655555755));
#11200=CARTESIAN_POINT('Ctrl Pts',(86.3855440365689,-4.3944270396494,0.602853429710152));
#11201=CARTESIAN_POINT('Ctrl Pts',(86.3918267665125,-4.40785559256641,0.475559283027399));
#11202=CARTESIAN_POINT('Ctrl Pts',(86.3929787870132,-4.41031789293486,0.452218240532605));
#11203=CARTESIAN_POINT('Ctrl Pts',(86.3941314875322,-4.41259496550383,0.428852521820395));
#11204=CARTESIAN_POINT('Ctrl Pts',(86.395284339639,-4.414686474794,0.405464948733126));
#11205=CARTESIAN_POINT('Ctrl Pts',(86.4018609031946,-4.4266177049082,0.272048129774276));
#11206=CARTESIAN_POINT('Ctrl Pts',(86.4084425476444,-4.43251295826403,0.137913142053602));
#11207=CARTESIAN_POINT('Ctrl Pts',(86.4149558832995,-4.43233551419456,0.00354868648530903));
#11208=CARTESIAN_POINT('',(87.6638081402417,-4.43299865229463,-0.00345669697483381));
#11209=CARTESIAN_POINT('Ctrl Pts',(86.4138081402417,-4.43299862504029,0.0034914740243378));
#11210=CARTESIAN_POINT('Ctrl Pts',(86.4194928266304,-4.43309858561255,-0.123424858811329));
#11211=CARTESIAN_POINT('Ctrl Pts',(86.4251775130191,-4.42774379894671,-0.250430731327767));
#11212=CARTESIAN_POINT('Ctrl Pts',(86.4308621994077,-4.41693837642756,-0.37702039578981));
#11213=CARTESIAN_POINT('Ctrl Pts',(86.4365232587161,-4.40617786414065,-0.503083919675518));
#11214=CARTESIAN_POINT('Ctrl Pts',(86.4421843180244,-4.39001197941783,-0.628734283778743));
#11215=CARTESIAN_POINT('Ctrl Pts',(86.4478453773327,-4.36849692902415,-0.753474340045224));
#11216=CARTESIAN_POINT('Ctrl Pts',(86.4535059960479,-4.34698355311981,-0.878204687949842));
#11217=CARTESIAN_POINT('Ctrl Pts',(86.4591666147631,-4.32012190817094,-1.00202447095209));
#11218=CARTESIAN_POINT('Ctrl Pts',(86.4648272334783,-4.2880196406845,-1.12444500136909));
#11219=CARTESIAN_POINT('Ctrl Pts',(86.470488723121,-4.25591243402978,-1.24688436707869));
#11220=CARTESIAN_POINT('Ctrl Pts',(86.4761502127638,-4.21856310384608,-1.36792366142097));
#11221=CARTESIAN_POINT('Ctrl Pts',(86.4818117024065,-4.17612950022084,-1.48708822784166));
#11222=CARTESIAN_POINT('Ctrl Pts',(86.4875141116701,-4.13338919869751,-1.60711408151878));
#11223=CARTESIAN_POINT('Ctrl Pts',(86.4932165209337,-4.08549096873137,-1.72523760539112));
#11224=CARTESIAN_POINT('Ctrl Pts',(86.4989189301973,-4.03264543254052,-1.84099424643591));
#11225=CARTESIAN_POINT('Ctrl Pts',(86.5045890089907,-3.98009951024224,-1.95609459178733));
#11226=CARTESIAN_POINT('Ctrl Pts',(86.510259087784,-3.92266247378685,-2.06885448967915));
#11227=CARTESIAN_POINT('Ctrl Pts',(86.5159291665774,-3.86058712465216,-2.17884282429227));
#11228=CARTESIAN_POINT('Ctrl Pts',(86.5216477410761,-3.79798085029511,-2.289771879849));
#11229=CARTESIAN_POINT('Ctrl Pts',(86.5273663155749,-3.73065677649181,-2.39788138712079));
#11230=CARTESIAN_POINT('Ctrl Pts',(86.5330848900736,-3.65891769727892,-2.50276053279956));
#11231=CARTESIAN_POINT('Ctrl Pts',(86.5388034645724,-3.58717861806602,-2.60763967847833));
#11232=CARTESIAN_POINT('Ctrl Pts',(86.5445220390712,-3.51102483123275,-2.70928816745404));
#11233=CARTESIAN_POINT('Ctrl Pts',(86.5502406135699,-3.43079859236735,-2.80733147643989));
#11234=CARTESIAN_POINT('Ctrl Pts',(86.5559517856266,-3.35067620282369,-2.90524787269393));
#11235=CARTESIAN_POINT('Ctrl Pts',(86.5616629576833,-3.26623502734388,-2.99988249200717));
#11236=CARTESIAN_POINT('Ctrl Pts',(86.56737412974,-3.1777737687688,-3.09083206831509));
#11237=CARTESIAN_POINT('Ctrl Pts',(86.5730783351364,-3.08942041791224,-3.18167070157926));
#11238=CARTESIAN_POINT('Ctrl Pts',(86.5787825405327,-2.99705701594037,-3.26883295112687));
#11239=CARTESIAN_POINT('Ctrl Pts',(86.584486745929,-2.90102301052981,-3.35194786540253));
#11240=CARTESIAN_POINT('Ctrl Pts',(86.5901854119731,-2.80508226371378,-3.43498206680926));
#11241=CARTESIAN_POINT('Ctrl Pts',(86.5958840780173,-2.70547830646356,-3.5139764940675));
#11242=CARTESIAN_POINT('Ctrl Pts',(86.6015827440614,-2.60258764965247,-3.58859673491971));
#11243=CARTESIAN_POINT('Ctrl Pts',(86.6072772930777,-2.49977132667532,-3.66316306603158));
#11244=CARTESIAN_POINT('Ctrl Pts',(86.612971842094,-2.39367335211702,-3.73336126685212));
#11245=CARTESIAN_POINT('Ctrl Pts',(86.6186663911103,-2.2847031770432,-3.79889726010176));
#11246=CARTESIAN_POINT('Ctrl Pts',(86.6243588077042,-2.17577380773753,-3.86440871226442));
#11247=CARTESIAN_POINT('Ctrl Pts',(86.6300512242981,-2.06397471796631,-3.92526122279219));
#11248=CARTESIAN_POINT('Ctrl Pts',(86.635743640892,-1.9497439167623,-3.98120429757736));
#11249=CARTESIAN_POINT('Ctrl Pts',(86.6414351262668,-1.83553180250814,-4.03713822066769));
#11250=CARTESIAN_POINT('Ctrl Pts',(86.6471266116415,-1.7188891264319,-4.08816413001825));
#11251=CARTESIAN_POINT('Ctrl Pts',(86.6528180970163,-1.60027756815729,-4.13407797517809));
#11252=CARTESIAN_POINT('Ctrl Pts',(86.6585099332263,-1.48165869841492,-4.17999465056463));
#11253=CARTESIAN_POINT('Ctrl Pts',(86.6642017694363,-1.36107107734571,-4.22079849092538));
#11254=CARTESIAN_POINT('Ctrl Pts',(86.6698936056463,-1.23899489838011,-4.25633417881962));
#11255=CARTESIAN_POINT('Ctrl Pts',(86.6755870746831,-1.11688369921225,-4.29188006089742));
#11256=CARTESIAN_POINT('Ctrl Pts',(86.6812805437199,-0.993283475745765,
-4.32215467252359));
#11257=CARTESIAN_POINT('Ctrl Pts',(86.6869740127567,-0.868687556312043,
-4.34705313166386));
#11258=CARTESIAN_POINT('Ctrl Pts',(86.6926735353827,-0.743959160086927,
-4.3719780641268));
#11259=CARTESIAN_POINT('Ctrl Pts',(86.6983730580086,-0.618233345895329,
-4.39151535277929));
#11260=CARTESIAN_POINT('Ctrl Pts',(86.7040725806346,-0.492011872695479,
-4.40561157129481));
#11261=CARTESIAN_POINT('Ctrl Pts',(86.7097755559243,-0.36571393689858,-4.41971632903466));
#11262=CARTESIAN_POINT('Ctrl Pts',(86.715478531214,-0.238920141515387,-4.42837342327373));
#11263=CARTESIAN_POINT('Ctrl Pts',(86.7211815065037,-0.112134030461784,
-4.43158154152808));
#11264=CARTESIAN_POINT('Ctrl Pts',(86.7268926498785,0.0148336699714674,
-4.43479425460909));
#11265=CARTESIAN_POINT('Ctrl Pts',(86.7326037932533,0.141793265893701,-4.43254241543301));
#11266=CARTESIAN_POINT('Ctrl Pts',(86.7383149366281,0.268244173801696,-4.42487672859046));
#11267=CARTESIAN_POINT('Ctrl Pts',(86.7408177826528,0.323659899062344,-4.42151732530085));
#11268=CARTESIAN_POINT('Ctrl Pts',(86.7433206286776,0.378978031091081,-4.41711884181208));
#11269=CARTESIAN_POINT('Ctrl Pts',(86.7458234747023,0.434157045701389,-4.41168864038112));
#11270=CARTESIAN_POINT('Ctrl Pts',(86.7515346465291,0.560068440393015,-4.39929762106958));
#11271=CARTESIAN_POINT('Ctrl Pts',(86.7572458183559,0.685643168840897,-4.38149285785934));
#11272=CARTESIAN_POINT('Ctrl Pts',(86.7629569901827,0.810380010705975,-4.35829935161046));
#11273=CARTESIAN_POINT('Ctrl Pts',(86.7686611953483,0.934964694775035,-4.33513413750639));
#11274=CARTESIAN_POINT('Ctrl Pts',(86.7743654005139,1.05871313659917,-4.30659333027187));
#11275=CARTESIAN_POINT('Ctrl Pts',(86.7800696056794,1.18112841818454,-4.27275375604035));
#11276=CARTESIAN_POINT('Ctrl Pts',(86.7857682714923,1.30342482230871,-4.23894704341418));
#11277=CARTESIAN_POINT('Ctrl Pts',(86.7914669373051,1.42439025976567,-4.19985190861399));
#11278=CARTESIAN_POINT('Ctrl Pts',(86.7971656031179,1.54353767212426,-4.15559628148996));
#11279=CARTESIAN_POINT('Ctrl Pts',(86.8028601519027,1.66259900587129,-4.11137262705306));
#11280=CARTESIAN_POINT('Ctrl Pts',(86.8085547006874,1.77984455576229,-4.06199603909253));
#11281=CARTESIAN_POINT('Ctrl Pts',(86.8142492494722,1.89480256774256,-4.00764422438871));
#11282=CARTESIAN_POINT('Ctrl Pts',(86.819941665835,2.00971753171319,-3.95331276265902));
#11283=CARTESIAN_POINT('Ctrl Pts',(86.8256340821978,2.12234630072409,-3.89400994890669));
#11284=CARTESIAN_POINT('Ctrl Pts',(86.8313264985605,2.2322375580017,-3.82996142077784));
#11285=CARTESIAN_POINT('Ctrl Pts',(86.8370179837046,2.34211083823889,-3.7659233703067));
#11286=CARTESIAN_POINT('Ctrl Pts',(86.8427094688486,2.44924715277715,-3.69714135060679));
#11287=CARTESIAN_POINT('Ctrl Pts',(86.8484009539927,2.55322071244419,-3.62388644876546));
#11288=CARTESIAN_POINT('Ctrl Pts',(86.8540927899725,2.65720068127262,-3.55062703132912));
#11289=CARTESIAN_POINT('Ctrl Pts',(86.8597846259523,2.75801718116145,-3.47289441328324));
#11290=CARTESIAN_POINT('Ctrl Pts',(86.8654764619321,2.8552747149209,-3.39100210886596));
#11291=CARTESIAN_POINT('Ctrl Pts',(86.8711699307396,2.9525601491309,-3.30908631185019));
#11292=CARTESIAN_POINT('Ctrl Pts',(86.8768633995471,3.04628428094089,-3.22300871157583));
#11293=CARTESIAN_POINT('Ctrl Pts',(86.8825568683545,3.13608630419801,-3.13312171685392));
#11294=CARTESIAN_POINT('Ctrl Pts',(86.8882563907536,3.2259838096287,-3.04313914961238));
#11295=CARTESIAN_POINT('Ctrl Pts',(86.8939559131527,3.31195059789399,-2.94933938358401));
#11296=CARTESIAN_POINT('Ctrl Pts',(86.8996554355518,3.39366401123373,-2.8521103728392));
#11297=CARTESIAN_POINT('Ctrl Pts',(86.9053584106158,3.47542692504215,-2.75482246256489));
#11298=CARTESIAN_POINT('Ctrl Pts',(86.9110613856797,3.55293108797739,-2.65410148502395));
#11299=CARTESIAN_POINT('Ctrl Pts',(86.9167643607437,3.62589622301142,-2.55036577375708));
#11300=CARTESIAN_POINT('Ctrl Pts',(86.9224755038964,3.69896586239475,-2.44648148696847));
#11301=CARTESIAN_POINT('Ctrl Pts',(86.9281866470491,3.76748327796095,-2.33957418003041));
#11302=CARTESIAN_POINT('Ctrl Pts',(86.9338977902018,3.83121312390325,-2.23008856309149));
#11303=CARTESIAN_POINT('Ctrl Pts',(86.936400638746,3.85914205999862,-2.18210764059535));
#11304=CARTESIAN_POINT('Ctrl Pts',(86.9389034872903,3.8861521373543,-2.13363182912283));
#11305=CARTESIAN_POINT('Ctrl Pts',(86.9414063358346,3.91222646030594,-2.08469976813979));
#11306=CARTESIAN_POINT('Ctrl Pts',(86.9471175075987,3.97172464182866,-1.97304322955773));
#11307=CARTESIAN_POINT('Ctrl Pts',(86.9528286793629,4.02653071554339,-1.85866527777414));
#11308=CARTESIAN_POINT('Ctrl Pts',(86.958539851127,4.07638759126769,-1.74199690176498));
#11309=CARTESIAN_POINT('Ctrl Pts',(86.9642440562285,4.12618365004387,-1.62547084142377));
#11310=CARTESIAN_POINT('Ctrl Pts',(86.9699482613299,4.17104236618554,-1.50666027923305));
#11311=CARTESIAN_POINT('Ctrl Pts',(86.9756524664314,4.21075216512944,-1.38602135764847));
#11312=CARTESIAN_POINT('Ctrl Pts',(86.9813511321787,4.25042340188367,-1.26549958853258));
#11313=CARTESIAN_POINT('Ctrl Pts',(86.987049797926,4.28495554685416,-1.14315337006245));
#11314=CARTESIAN_POINT('Ctrl Pts',(86.9927484636733,4.3141850217428,-1.01945897326479));
#11315=CARTESIAN_POINT('Ctrl Pts',(86.9984430123912,4.34339337965205,-0.895853940098765));
#11316=CARTESIAN_POINT('Ctrl Pts',(87.0041375611091,4.36730660072948,-0.770903054289988));
#11317=CARTESIAN_POINT('Ctrl Pts',(87.009832109827,4.38581101758013,-0.645097448508964));
#11318=CARTESIAN_POINT('Ctrl Pts',(87.0155245261213,4.40430850512718,-0.519338952844576));
#11319=CARTESIAN_POINT('Ctrl Pts',(87.0212169424155,4.41740115767103,-0.392726767871859));
#11320=CARTESIAN_POINT('Ctrl Pts',(87.0269093587097,4.42502652826775,-0.265761592647671));
#11321=CARTESIAN_POINT('Ctrl Pts',(87.0326008437842,4.43265065143359,-0.138817187598398));
#11322=CARTESIAN_POINT('Ctrl Pts',(87.0382923288586,4.434809247751,-0.0115203054542955));
#11323=CARTESIAN_POINT('Ctrl Pts',(87.0439838139331,4.43149184790243,0.115624400427719));
#11324=CARTESIAN_POINT('Ctrl Pts',(87.0496756498424,4.4281742435625,0.242776943771324));
#11325=CARTESIAN_POINT('Ctrl Pts',(87.0553674857517,4.41937998211374,0.369776893159533));
#11326=CARTESIAN_POINT('Ctrl Pts',(87.061059321661,4.4051506982053,0.496121281645249));
#11327=CARTESIAN_POINT('Ctrl Pts',(87.066752790397,4.39091733231779,0.622501914762336));
#11328=CARTESIAN_POINT('Ctrl Pts',(87.0724462591331,4.371245886927,0.74822621636346));
#11329=CARTESIAN_POINT('Ctrl Pts',(87.0781397278691,4.34622959976409,0.872798525511165));
#11330=CARTESIAN_POINT('Ctrl Pts',(87.083839250196,4.32118671398931,0.997503286388406));
#11331=CARTESIAN_POINT('Ctrl Pts',(87.0895387725228,4.29078771852967,1.12105321755604));
#11332=CARTESIAN_POINT('Ctrl Pts',(87.0952382948496,4.25517658371521,1.24296469837311));
#11333=CARTESIAN_POINT('Ctrl Pts',(87.1009412698406,4.21954387634003,1.36495003088954));
#11334=CARTESIAN_POINT('Ctrl Pts',(87.1066442448317,4.17869286775462,1.48529455843778));
#11335=CARTESIAN_POINT('Ctrl Pts',(87.1123472198227,4.13281630837234,1.60353308704611));
#11336=CARTESIAN_POINT('Ctrl Pts',(87.1180583629022,4.08687404226776,1.7219409628389));
#11337=CARTESIAN_POINT('Ctrl Pts',(87.1237695059817,4.03589201286711,1.83823645205888));
#11338=CARTESIAN_POINT('Ctrl Pts',(87.1294806490612,3.98010983348217,1.95197712932774));
#11339=CARTESIAN_POINT('Ctrl Pts',(87.1319834983631,3.95566387112538,2.00182280308249));
#11340=CARTESIAN_POINT('Ctrl Pts',(87.134486347665,3.93029659796724,2.0511781665134));
#11341=CARTESIAN_POINT('Ctrl Pts',(87.136989196967,3.90403080308594,2.10000773535627));
#11342=CARTESIAN_POINT('Ctrl Pts',(87.1427003695097,3.84409571773264,2.21143038179008));
#11343=CARTESIAN_POINT('Ctrl Pts',(87.1484115420525,3.779294315079,2.32045700289408));
#11344=CARTESIAN_POINT('Ctrl Pts',(87.1541227145952,3.70984273353467,2.42663468458687));
#11345=CARTESIAN_POINT('Ctrl Pts',(87.1598269204775,3.64047587112314,2.53268284754278));
#11346=CARTESIAN_POINT('Ctrl Pts',(87.1655311263598,3.56647033164159,2.63588865379617));
#11347=CARTESIAN_POINT('Ctrl Pts',(87.1712353322421,3.48808842249057,2.73582312236871));
#11348=CARTESIAN_POINT('Ctrl Pts',(87.1769339987716,3.40978262999094,2.83566054460506));
#11349=CARTESIAN_POINT('Ctrl Pts',(87.182632665301,3.32710916944895,2.93223263822301));
#11350=CARTESIAN_POINT('Ctrl Pts',(87.1883313318305,3.24037371077588,3.02513920580732));
#11351=CARTESIAN_POINT('Ctrl Pts',(87.194025881331,3.15370091455087,3.11797865259635));
#11352=CARTESIAN_POINT('Ctrl Pts',(87.1997204308315,3.06297223241824,3.20715755325056));
#11353=CARTESIAN_POINT('Ctrl Pts',(87.205414980332,2.96853337508941,3.29230900751741));
#11354=CARTESIAN_POINT('Ctrl Pts',(87.2111073974065,2.87412988208054,3.37742857529855));
#11355=CARTESIAN_POINT('Ctrl Pts',(87.2167998144811,2.77601927231698,3.45852342853764));
#11356=CARTESIAN_POINT('Ctrl Pts',(87.2224922315556,2.67458361653639,3.53526398988182));
#11357=CARTESIAN_POINT('Ctrl Pts',(87.2281837174087,2.57316455459554,3.61199199725209));
#11358=CARTESIAN_POINT('Ctrl Pts',(87.2338752032619,2.46842184679726,3.68436688885085));
#11359=CARTESIAN_POINT('Ctrl Pts',(87.239566689115,2.36076967320276,3.75210015192641));
#11360=CARTESIAN_POINT('Ctrl Pts',(87.2452585258005,2.253110863754,3.81983759018995));
#11361=CARTESIAN_POINT('Ctrl Pts',(87.250950362486,2.14254256967276,3.88293261829609));
#11362=CARTESIAN_POINT('Ctrl Pts',(87.2566421991715,2.02950645605981,3.94114102067048));
#11363=CARTESIAN_POINT('Ctrl Pts',(87.2623356686804,1.91643791565405,3.99936612135254));
#11364=CARTESIAN_POINT('Ctrl Pts',(87.2680291381893,1.80090050209572,4.05270162490488));
#11365=CARTESIAN_POINT('Ctrl Pts',(87.2737226076982,1.68335841105118,4.10095031181106));
#11366=CARTESIAN_POINT('Ctrl Pts',(87.2794221307887,1.56569134337505,4.14925029913494));
#11367=CARTESIAN_POINT('Ctrl Pts',(87.2851216538792,1.44601571207244,4.19245251931413));
#11368=CARTESIAN_POINT('Ctrl Pts',(87.2908211769697,1.32481382075879,4.23040864933005));
#11369=CARTESIAN_POINT('Ctrl Pts',(87.2965241527202,1.20353850770115,4.26838777242991));
#11370=CARTESIAN_POINT('Ctrl Pts',(87.3022271284708,1.08073547782594,4.30111437183663));
#11371=CARTESIAN_POINT('Ctrl Pts',(87.3079301042213,0.956898745256767,4.32849093695782));
#11372=CARTESIAN_POINT('Ctrl Pts',(87.3136412480473,0.832884647779103,4.35590671210877));
#11373=CARTESIAN_POINT('Ctrl Pts',(87.3193523918732,0.707834283578074,4.37795708345785));
#11374=CARTESIAN_POINT('Ctrl Pts',(87.3250635356992,0.58224870086875,4.39459616464774));
#11375=CARTESIAN_POINT('Ctrl Pts',(87.3275663764992,0.527212314134499,4.40188804391854));
#11376=CARTESIAN_POINT('Ctrl Pts',(87.3300692172993,0.472073164742458,4.40814134586292));
#11377=CARTESIAN_POINT('Ctrl Pts',(87.3325720580993,0.416873418278865,4.41335536220827));
#11378=CARTESIAN_POINT('Ctrl Pts',(87.338283229234,0.290914468495186,4.42525309843155));
#11379=CARTESIAN_POINT('Ctrl Pts',(87.3439944003688,0.164251468113924,4.43177252013408));
#11380=CARTESIAN_POINT('Ctrl Pts',(87.3497055715035,0.0373811785528921,
4.43284238920018));
#11381=CARTESIAN_POINT('Ctrl Pts',(87.3554097759797,-0.089334350807393,
4.43391095320778));
#11382=CARTESIAN_POINT('Ctrl Pts',(87.3611139804558,-0.216256270566662,
4.42954318637758));
#11383=CARTESIAN_POINT('Ctrl Pts',(87.366818184932,-0.342882139069563,4.41971954299219));
#11384=CARTESIAN_POINT('Ctrl Pts',(87.3725168500588,-0.469385041272681,
4.40990543934059));
#11385=CARTESIAN_POINT('Ctrl Pts',(87.3782155151857,-0.595592068574799,
4.39464603248982));
#11386=CARTESIAN_POINT('Ctrl Pts',(87.3839141803125,-0.721000691778549,
4.37397382279031));
#11387=CARTESIAN_POINT('Ctrl Pts',(87.3896087284155,-0.846318713011158,
4.35331654781298));
#11388=CARTESIAN_POINT('Ctrl Pts',(87.3953032765185,-0.970839085673708,
4.32725431776791));
#11389=CARTESIAN_POINT('Ctrl Pts',(87.4009978246215,-1.09406479104341,4.2958714171864));
#11390=CARTESIAN_POINT('Ctrl Pts',(87.4066902403111,-1.2172443526039,4.26450026842708));
#11391=CARTESIAN_POINT('Ctrl Pts',(87.4123826560007,-1.33912982465032,4.22781250905882));
#11392=CARTESIAN_POINT('Ctrl Pts',(87.4180750716904,-1.45923509001766,4.18594337659519));
#11393=CARTESIAN_POINT('Ctrl Pts',(87.4237665561668,-1.57932070755703,4.14408109343588));
#11394=CARTESIAN_POINT('Ctrl Pts',(87.4294580406433,-1.69762632090548,4.09703925450177));
#11395=CARTESIAN_POINT('Ctrl Pts',(87.4351495251197,-1.813682185152,4.04500258729982));
#11396=CARTESIAN_POINT('Ctrl Pts',(87.4408413604383,-1.92974520346841,3.99296271238445));
#11397=CARTESIAN_POINT('Ctrl Pts',(87.4465331957568,-2.04355783262413,3.93592756013947));
#11398=CARTESIAN_POINT('Ctrl Pts',(87.4522250310753,-2.15467195407877,3.87412929189339));
#11399=CARTESIAN_POINT('Ctrl Pts',(87.4579184992284,-2.26581795118839,3.81231329538513));
#11400=CARTESIAN_POINT('Ctrl Pts',(87.4636119673815,-2.3742635518877,3.74573165854805));
#11401=CARTESIAN_POINT('Ctrl Pts',(87.4693054355345,-2.47958725703953,3.67466134966573));
#11402=CARTESIAN_POINT('Ctrl Pts',(87.4750049572933,-2.5850229480959,3.60351547495695));
#11403=CARTESIAN_POINT('Ctrl Pts',(87.4807044790521,-2.68732978494485,3.52787162263622));
#11404=CARTESIAN_POINT('Ctrl Pts',(87.4864040008109,-2.78611692151813,3.44804894101438));
#11405=CARTESIAN_POINT('Ctrl Pts',(87.4921069752416,-2.88496390163468,3.36817790418893));
#11406=CARTESIAN_POINT('Ctrl Pts',(87.4978099496723,-2.98028663503646,3.28412325865201));
#11407=CARTESIAN_POINT('Ctrl Pts',(87.5035129241031,-3.07173007020539,3.19624207090077));
#11408=CARTESIAN_POINT('Ctrl Pts',(87.5092240666389,-3.16330447555466,3.10823501501051));
#11409=CARTESIAN_POINT('Ctrl Pts',(87.5149352091748,-3.25098821335561,3.01639076155084));
#11410=CARTESIAN_POINT('Ctrl Pts',(87.5206463517106,-3.3344652950368,2.92110085347889));
#11411=CARTESIAN_POINT('Ctrl Pts',(87.523149207551,-3.37104836052882,2.87934092515465));
#11412=CARTESIAN_POINT('Ctrl Pts',(87.5256520633914,-3.40682406325378,2.83691963875481));
#11413=CARTESIAN_POINT('Ctrl Pts',(87.5281549192318,-3.44176843506732,2.79387169343445));
#11414=CARTESIAN_POINT('Ctrl Pts',(87.5338375449392,-3.52110811672034,2.69613319935708));
#11415=CARTESIAN_POINT('Ctrl Pts',(87.5395201706467,-3.5964119446753,2.59485124280539));
#11416=CARTESIAN_POINT('Ctrl Pts',(87.5452027963541,-3.66734576426601,2.49039435538232));
#11417=CARTESIAN_POINT('Ctrl Pts',(87.5508788258846,-3.7381972465619,2.38605871756327));
#11418=CARTESIAN_POINT('Ctrl Pts',(87.5565548554151,-3.80468858180469,2.27855580652901));
#11419=CARTESIAN_POINT('Ctrl Pts',(87.5622308849455,-3.86652512646031,2.16828790672527));
#11420=CARTESIAN_POINT('Ctrl Pts',(87.5679016376123,-3.92830418321563,2.05812252025028));
#11421=CARTESIAN_POINT('Ctrl Pts',(87.573572390279,-3.98543685943425,1.94519760652178));
#11422=CARTESIAN_POINT('Ctrl Pts',(87.5792431429458,-4.03767152406703,1.82994471603331));
#11423=CARTESIAN_POINT('Ctrl Pts',(87.584909933831,-4.08986969577898,1.71477234515067));
#11424=CARTESIAN_POINT('Ctrl Pts',(87.5905767247163,-4.13717649718736,1.59727559882149));
#11425=CARTESIAN_POINT('Ctrl Pts',(87.5962435156015,-4.17938628647332,1.4779104399248));
#11426=CARTESIAN_POINT('Ctrl Pts',(87.6019084037978,-4.22158190334661,1.3585853592261));
#11427=CARTESIAN_POINT('Ctrl Pts',(87.6075732919941,-4.2586837726074,1.2373934914744));
#11428=CARTESIAN_POINT('Ctrl Pts',(87.6132381801904,-4.29053459634209,1.11481024286272));
#11429=CARTESIAN_POINT('Ctrl Pts',(87.618901742379,-4.32237796460081,0.992255687903418));
#11430=CARTESIAN_POINT('Ctrl Pts',(87.6245653045676,-4.34897263461876,0.86831079114068));
#11431=CARTESIAN_POINT('Ctrl Pts',(87.6302288667562,-4.37021155684452,0.743464826621006));
#11432=CARTESIAN_POINT('Ctrl Pts',(87.6358946104868,-4.39145866006998,0.618570772806246));
#11433=CARTESIAN_POINT('Ctrl Pts',(87.6415603542174,-4.40734582223827,0.49277535519587));
#11434=CARTESIAN_POINT('Ctrl Pts',(87.647226097948,-4.41781739133026,0.366576727111689));
#11435=CARTESIAN_POINT('Ctrl Pts',(87.6527534453792,-4.42803317292469,0.243460734589467));
#11436=CARTESIAN_POINT('Ctrl Pts',(87.6582807928105,-4.43309488937622,0.119961368332007));
#11437=CARTESIAN_POINT('Ctrl Pts',(87.6638081402417,-4.43299865229463,-0.00345669697483381));
#11438=CARTESIAN_POINT('',(88.9113509797465,-4.43441641653233,0.00189839995018913));
#11439=CARTESIAN_POINT('Ctrl Pts',(87.6650202097439,-4.43229847675382,-0.0034084650769976));
#11440=CARTESIAN_POINT('Ctrl Pts',(87.6704932507814,-4.43247486644053,-0.136375602761746));
#11441=CARTESIAN_POINT('Ctrl Pts',(87.6758922634644,-4.42670672871812,-0.269126783054866));
#11442=CARTESIAN_POINT('Ctrl Pts',(87.6812939294348,-4.41502948433978,-0.401177373261769));
#11443=CARTESIAN_POINT('Ctrl Pts',(87.6820309487695,-4.41343620646417,-0.41919474765439));
#11444=CARTESIAN_POINT('Ctrl Pts',(87.6827680174995,-4.4117328828111,-0.437199149181645));
#11445=CARTESIAN_POINT('Ctrl Pts',(87.6835053304052,-4.40991956510187,-0.455189411580503));
#11446=CARTESIAN_POINT('Ctrl Pts',(87.6887178317711,-4.39710014886352,-0.582373225401012));
#11447=CARTESIAN_POINT('Ctrl Pts',(87.6939430646484,-4.3787846963171,-0.708848125842272));
#11448=CARTESIAN_POINT('Ctrl Pts',(87.6992680587665,-4.35502730272325,-0.834168868242767));
#11449=CARTESIAN_POINT('Ctrl Pts',(87.7002866233693,-4.35048298969048,-0.858140213445957));
#11450=CARTESIAN_POINT('Ctrl Pts',(87.7013088380383,-4.34573953157213,-0.882069479404934));
#11451=CARTESIAN_POINT('Ctrl Pts',(87.7023353118557,-4.34079724846068,-0.905953759614343));
#11452=CARTESIAN_POINT('Ctrl Pts',(87.7074381184735,-4.31622817076992,-1.02468729284592));
#11453=CARTESIAN_POINT('Ctrl Pts',(87.7126470002665,-4.28674658211013,-1.14230537053208));
#11454=CARTESIAN_POINT('Ctrl Pts',(87.7180446809552,-4.25242531284092,-1.25841504416937));
#11455=CARTESIAN_POINT('Ctrl Pts',(87.7189358598286,-4.2467587327216,-1.27758522004874));
#11456=CARTESIAN_POINT('Ctrl Pts',(87.7198321852358,-4.24096022935233,-1.2967143930399));
#11457=CARTESIAN_POINT('Ctrl Pts',(87.7207340294856,-4.23503013026258,-1.31580093141052));
#11458=CARTESIAN_POINT('Ctrl Pts',(87.720736064821,-4.23501674686482,-1.31584400703725));
#11459=CARTESIAN_POINT('Ctrl Pts',(87.7207381001845,-4.23500336279679,-1.31588708244684));
#11460=CARTESIAN_POINT('Ctrl Pts',(87.720740135576,-4.23498997805851,-1.31593015763928));
#11461=CARTESIAN_POINT('Ctrl Pts',(87.7259254174359,-4.20089155617928,-1.42566678853588));
#11462=CARTESIAN_POINT('Ctrl Pts',(87.7313001131529,-4.16237657502355,-1.53418712737575));
#11463=CARTESIAN_POINT('Ctrl Pts',(87.736787344819,-4.11958680619465,-1.64112867881909));
#11464=CARTESIAN_POINT('Ctrl Pts',(87.7373441981263,-4.11524442997581,-1.65198128360064));
#11465=CARTESIAN_POINT('Ctrl Pts',(87.737902210388,-4.11085806677358,-1.66281760494681));
#11466=CARTESIAN_POINT('Ctrl Pts',(87.7384613012579,-4.10642789009959,-1.67363724810316));
#11467=CARTESIAN_POINT('Ctrl Pts',(87.7445222703657,-4.05840141460399,-1.79093038676529));
#11468=CARTESIAN_POINT('Ctrl Pts',(87.7507094639741,-4.005221102134,-1.90626706198716));
#11469=CARTESIAN_POINT('Ctrl Pts',(87.7569313067568,-3.94711672539678,-2.01919391889636));
#11470=CARTESIAN_POINT('Ctrl Pts',(87.7631471075195,-3.88906877371245,-2.13201111274348));
#11471=CARTESIAN_POINT('Ctrl Pts',(87.7693971393272,-3.82610663410772,-2.24242336510873));
#11472=CARTESIAN_POINT('Ctrl Pts',(87.7756074729833,-3.75849115474214,-2.35000689449741));
#11473=CARTESIAN_POINT('Ctrl Pts',(87.7803266115315,-3.70711117537159,-2.43175799014097));
#11474=CARTESIAN_POINT('Ctrl Pts',(87.7850227077351,-3.65304257006595,-2.51187816833776));
#11475=CARTESIAN_POINT('Ctrl Pts',(87.7895788522303,-3.59628569676082,-2.59009042555527));
#11476=CARTESIAN_POINT('Ctrl Pts',(87.7910142113194,-3.57840511943216,-2.6147302661911));
#11477=CARTESIAN_POINT('Ctrl Pts',(87.792435680341,-3.56025796526518,-2.63918043531533));
#11478=CARTESIAN_POINT('Ctrl Pts',(87.7938396038648,-3.5418449179304,-2.66343143601119));
#11479=CARTESIAN_POINT('Ctrl Pts',(87.7987508798228,-3.47743146865384,-2.7482675076743));
#11480=CARTESIAN_POINT('Ctrl Pts',(87.8035384099442,-3.40989265204633,-2.83075774095742));
#11481=CARTESIAN_POINT('Ctrl Pts',(87.8083050895569,-3.33957594672189,-2.91081530851117));
#11482=CARTESIAN_POINT('Ctrl Pts',(87.8092240279107,-3.32602002883153,-2.92624910631573));
#11483=CARTESIAN_POINT('Ctrl Pts',(87.8101421913435,-3.31236076197933,-2.94159260545349));
#11484=CARTESIAN_POINT('Ctrl Pts',(87.8110603170918,-3.29860047779486,-2.9568453406073));
#11485=CARTESIAN_POINT('Ctrl Pts',(87.8186088511059,-3.18546785581371,-3.08224841348005));
#11486=CARTESIAN_POINT('Ctrl Pts',(87.826154919603,-3.06550846397169,-3.2015208266937));
#11487=CARTESIAN_POINT('Ctrl Pts',(87.8337038723534,-2.93944514446068,-3.3139489700716));
#11488=CARTESIAN_POINT('Ctrl Pts',(87.8375152217357,-2.87579772595896,-3.37071219922264));
#11489=CARTESIAN_POINT('Ctrl Pts',(87.8413272904779,-2.81059401751932,-3.42572993898006));
#11490=CARTESIAN_POINT('Ctrl Pts',(87.8451406948563,-2.74392526922058,-3.47890548267059));
#11491=CARTESIAN_POINT('Ctrl Pts',(87.8505406971192,-2.64951844635391,-3.55420514348822));
#11492=CARTESIAN_POINT('Ctrl Pts',(87.8557777363124,-2.55199162266314,-3.62558803805759));
#11493=CARTESIAN_POINT('Ctrl Pts',(87.8607660921093,-2.45160000857682,-3.6925894509802));
#11494=CARTESIAN_POINT('Ctrl Pts',(87.8610293819821,-2.44630124954955,-3.69612584537723));
#11495=CARTESIAN_POINT('Ctrl Pts',(87.8612919790672,-2.44099452043001,-3.69965002813721));
#11496=CARTESIAN_POINT('Ctrl Pts',(87.8615538707602,-2.43567986237023,-3.70316192913125));
#11497=CARTESIAN_POINT('Ctrl Pts',(87.8667831820891,-2.32955965183829,-3.77328566402855));
#11498=CARTESIAN_POINT('Ctrl Pts',(87.8719528300163,-2.22049027771163,-3.83883161504912));
#11499=CARTESIAN_POINT('Ctrl Pts',(87.8771271699654,-2.10889404994695,-3.89952825585647));
#11500=CARTESIAN_POINT('Ctrl Pts',(87.8823046444025,-1.9972302199301,-3.96026166519713));
#11501=CARTESIAN_POINT('Ctrl Pts',(87.8874871793512,-1.88303635926708,-4.01613950495026));
#11502=CARTESIAN_POINT('Ctrl Pts',(87.8927552908126,-1.76676550402013,-4.06692343977424));
#11503=CARTESIAN_POINT('Ctrl Pts',(87.8976222086898,-1.65934926801978,-4.11383991868457));
#11504=CARTESIAN_POINT('Ctrl Pts',(87.9025626112088,-1.55015983571756,-4.15640893974705));
#11505=CARTESIAN_POINT('Ctrl Pts',(87.9076474056353,-1.43958038938607,-4.19447285018349));
#11506=CARTESIAN_POINT('Ctrl Pts',(87.9080744423271,-1.43029358701345,-4.1976695745792));
#11507=CARTESIAN_POINT('Ctrl Pts',(87.9085024974378,-1.42099696242394,-4.20083454811592));
#11508=CARTESIAN_POINT('Ctrl Pts',(87.9089316129689,-1.41169073228986,-4.20396769064737));
#11509=CARTESIAN_POINT('Ctrl Pts',(87.9113568433636,-1.35909475162497,-4.22167525876358));
#11510=CARTESIAN_POINT('Ctrl Pts',(87.9138160196822,-1.30619305549409,-4.23836575694949));
#11511=CARTESIAN_POINT('Ctrl Pts',(87.9163168496607,-1.25302836710145,-4.2540254365958));
#11512=CARTESIAN_POINT('Ctrl Pts',(87.9163188850285,-1.25298509758774,-4.25403818164789));
#11513=CARTESIAN_POINT('Ctrl Pts',(87.916320920424,-1.2529418278997,-4.25405092601733));
#11514=CARTESIAN_POINT('Ctrl Pts',(87.916322955847,-1.25289855803742,-4.25406366970412));
#11515=CARTESIAN_POINT('Ctrl Pts',(87.921508234785,-1.14266775958701,-4.28652845456093));
#11516=CARTESIAN_POINT('Ctrl Pts',(87.9268829273223,-1.0310004726749,-4.31464332669523));
#11517=CARTESIAN_POINT('Ctrl Pts',(87.932370155382,-0.918276977479303,-4.33832528957188));
#11518=CARTESIAN_POINT('Ctrl Pts',(87.9329270039934,-0.906837700472616,
-4.34072855548319));
#11519=CARTESIAN_POINT('Ctrl Pts',(87.9334850115367,-0.895387586959527,
-4.34308618704253));
#11520=CARTESIAN_POINT('Ctrl Pts',(87.9340440976675,-0.883927061654988,
-4.34539810978408));
#11521=CARTESIAN_POINT('Ctrl Pts',(87.9401050581766,-0.759685397524938,
-4.37046128281655));
#11522=CARTESIAN_POINT('Ctrl Pts',(87.9462922425437,-0.6342144573966,-4.39015059275159));
#11523=CARTESIAN_POINT('Ctrl Pts',(87.9525140754823,-0.508018926972272,
-4.40440590351206));
#11524=CARTESIAN_POINT('Ctrl Pts',(87.9587298664203,-0.38194594459413,-4.41864737098922));
#11525=CARTESIAN_POINT('Ctrl Pts',(87.9649798878039,-0.255149789147666,
-4.42746576246532));
#11526=CARTESIAN_POINT('Ctrl Pts',(87.9711902104774,-0.128127764278676,
-4.4308432002155));
#11527=CARTESIAN_POINT('Ctrl Pts',(87.9759093388396,-0.0316056877795214,
-4.43340966304138));
#11528=CARTESIAN_POINT('Ctrl Pts',(87.9806054245533,0.0650497834022098,
-4.43283435754993));
#11529=CARTESIAN_POINT('Ctrl Pts',(87.9851615579815,0.161607923050945,-4.42896399908761));
#11530=CARTESIAN_POINT('Ctrl Pts',(87.98659691595,0.192027465706768,-4.42774468671513));
#11531=CARTESIAN_POINT('Ctrl Pts',(87.988018383748,0.222436960284434,-4.42619836172543));
#11532=CARTESIAN_POINT('Ctrl Pts',(87.9894223059185,0.252828124164767,-4.42432032756967));
#11533=CARTESIAN_POINT('Ctrl Pts',(87.9943335722267,0.359143917427554,-4.41775050050313));
#11534=CARTESIAN_POINT('Ctrl Pts',(87.9991210925003,0.465240279733896,-4.40727905639325));
#11535=CARTESIAN_POINT('Ctrl Pts',(88.0038877622561,0.570852296194735,-4.39314703482003));
#11536=CARTESIAN_POINT('Ctrl Pts',(88.0048066973714,0.591212546746425,-4.39042261472395));
#11537=CARTESIAN_POINT('Ctrl Pts',(88.0057248575676,0.611554949592072,-4.38756212091687));
#11538=CARTESIAN_POINT('Ctrl Pts',(88.0066429800793,0.631877824749012,-4.38456723584004));
#11539=CARTESIAN_POINT('Ctrl Pts',(88.0141915051284,0.798966345326882,-4.35994419835522));
#11540=CARTESIAN_POINT('Ctrl Pts',(88.0217375646512,0.964737827260598,-4.32624069876181));
#11541=CARTESIAN_POINT('Ctrl Pts',(88.0292865084281,1.12819761612251,-4.28366264960545));
#11542=CARTESIAN_POINT('Ctrl Pts',(88.0330978408085,1.21072566303948,-4.26216572205602));
#11543=CARTESIAN_POINT('Ctrl Pts',(88.0369098925447,1.29266394782887,-4.23840586407211));
#11544=CARTESIAN_POINT('Ctrl Pts',(88.0407232799098,1.37388139772529,-4.21240539787271));
#11545=CARTESIAN_POINT('Ctrl Pts',(88.0461234659674,1.4888944552994,-4.17558580898191));
#11546=CARTESIAN_POINT('Ctrl Pts',(88.0513606683849,1.60237763358752,-4.13399772909822));
#11547=CARTESIAN_POINT('Ctrl Pts',(88.0563491708192,1.71380263773121,-4.08759591053028));
#11548=CARTESIAN_POINT('Ctrl Pts',(88.0566122778055,1.71967949103894,-4.08514855427455));
#11549=CARTESIAN_POINT('Ctrl Pts',(88.0568746929605,1.72555060835203,-4.08268781300049));
#11550=CARTESIAN_POINT('Ctrl Pts',(88.0571364037082,1.73141590866033,-4.0802136820861));
#11551=CARTESIAN_POINT('Ctrl Pts',(88.0623656985315,1.84861164791632,-4.03077757714906));
#11552=CARTESIAN_POINT('Ctrl Pts',(88.0675353291997,1.96363279254374,-3.9763490223034));
#11553=CARTESIAN_POINT('Ctrl Pts',(88.0727096511316,2.07601922845231,-3.9171289283953));
#11554=CARTESIAN_POINT('Ctrl Pts',(88.0778871076421,2.18847374750829,-3.857872959247));
#11555=CARTESIAN_POINT('Ctrl Pts',(88.0830696239014,2.29829011002147,-3.79381933644778));
#11556=CARTESIAN_POINT('Ctrl Pts',(88.0883377160113,2.40501878853675,-3.72521294407968));
#11557=CARTESIAN_POINT('Ctrl Pts',(88.0932046213541,2.50361964153341,-3.66183120917371));
#11558=CARTESIAN_POINT('Ctrl Pts',(88.0981450109309,2.5995855754952,-3.59456338160326));
#11559=CARTESIAN_POINT('Ctrl Pts',(88.1032297924543,2.69257293712625,-3.52364094582055));
#11560=CARTESIAN_POINT('Ctrl Pts',(88.1036568222865,2.70038219643332,-3.51768474185905));
#11561=CARTESIAN_POINT('Ctrl Pts',(88.1040848705103,2.70817047837773,-3.51170276042284));
#11562=CARTESIAN_POINT('Ctrl Pts',(88.1045139791259,2.71593759613605,-3.5056951373899));
#11563=CARTESIAN_POINT('Ctrl Pts',(88.1069393433764,2.75983811235644,-3.47173945902755));
#11564=CARTESIAN_POINT('Ctrl Pts',(88.1093986574765,2.80306162344316,-3.43696535989147));
#11565=CARTESIAN_POINT('Ctrl Pts',(88.1118996305585,2.84557299403375,-3.4014007773705));
#11566=CARTESIAN_POINT('Ctrl Pts',(88.1119016659844,2.84560759206534,-3.40137183300733));
#11567=CARTESIAN_POINT('Ctrl Pts',(88.111903701438,2.84564218962542,-3.40134288812056));
#11568=CARTESIAN_POINT('Ctrl Pts',(88.1119057369191,2.84567678671398,-3.40131394271026));
#11569=CARTESIAN_POINT('Ctrl Pts',(88.1170910069154,2.93381086180585,-3.3275771899429));
#11570=CARTESIAN_POINT('Ctrl Pts',(88.1224656925541,3.01912129529592,-3.25023320982176));
#11571=CARTESIAN_POINT('Ctrl Pts',(88.1279529163455,3.10132817503194,-3.16955246187055));
#11572=CARTESIAN_POINT('Ctrl Pts',(88.1285097837992,3.10967088849377,-3.16136462693259));
#11573=CARTESIAN_POINT('Ctrl Pts',(88.129067810292,3.11798163009313,-3.15314246987529));
#11574=CARTESIAN_POINT('Ctrl Pts',(88.129626915472,3.12626010235041,-3.14488630290015));
#11575=CARTESIAN_POINT('Ctrl Pts',(88.1356878919153,3.21600283258085,-3.05538537295072));
#11576=CARTESIAN_POINT('Ctrl Pts',(88.1418750959406,3.30195485866196,-2.96188192063048));
#11577=CARTESIAN_POINT('Ctrl Pts',(88.1480969516428,3.38378631555431,-2.86476261645715));
#11578=CARTESIAN_POINT('Ctrl Pts',(88.15431276521,3.46553830472435,-2.76773762625779));
#11579=CARTESIAN_POINT('Ctrl Pts',(88.1605628123134,3.54317802963119,-2.66710402004398));
#11580=CARTESIAN_POINT('Ctrl Pts',(88.1667731628852,3.61641488684677,-2.56326575450496));
#11581=CARTESIAN_POINT('Ctrl Pts',(88.1714920014503,3.67206277696543,-2.48436585887157));
#11582=CARTESIAN_POINT('Ctrl Pts',(88.1761878016584,3.72517030285907,-2.40361326898927));
#11583=CARTESIAN_POINT('Ctrl Pts',(88.1807436466793,3.77548197922601,-2.32111496719795));
#11584=CARTESIAN_POINT('Ctrl Pts',(88.1821793085198,3.79133645925306,-2.29511766850974));
#11585=CARTESIAN_POINT('Ctrl Pts',(88.1836010722604,3.8069131011855,-2.26894734746114));
#11586=CARTESIAN_POINT('Ctrl Pts',(88.1850052792021,3.82220339736006,-2.24260829524297));
#11587=CARTESIAN_POINT('Ctrl Pts',(88.1899168034355,3.87568458874708,-2.1504816368349));
#11588=CARTESIAN_POINT('Ctrl Pts',(88.1947045967808,3.92579673910117,-2.05637417839698));
#11589=CARTESIAN_POINT('Ctrl Pts',(88.1994715479029,3.97259354455629,-1.96064006644912));
#11590=CARTESIAN_POINT('Ctrl Pts',(88.200390202769,3.98161191121198,-1.9421908301261));
#11591=CARTESIAN_POINT('Ctrl Pts',(88.2013080835879,3.99050721394496,-1.92368104026898));
#11592=CARTESIAN_POINT('Ctrl Pts',(88.2022259267408,3.99927992078292,-1.90511302553519));
#11593=CARTESIAN_POINT('Ctrl Pts',(88.2097744805054,4.0714286850071,-1.75240539015164));
#11594=CARTESIAN_POINT('Ctrl Pts',(88.2173205684079,4.13529019115885,-1.59575923575179));
#11595=CARTESIAN_POINT('Ctrl Pts',(88.2248695402585,4.19048433181604,-1.43611651446079));
#11596=CARTESIAN_POINT('Ctrl Pts',(88.2286808534316,4.21835066375185,-1.35551634549971));
#11597=CARTESIAN_POINT('Ctrl Pts',(88.2324928858723,4.24400676709187,-1.27415234284282));
#11598=CARTESIAN_POINT('Ctrl Pts',(88.236306253849,4.2673985488282,-1.19214596267452));
#11599=CARTESIAN_POINT('Ctrl Pts',(88.2416972545699,4.30046777083157,-1.07621263095802));
#11600=CARTESIAN_POINT('Ctrl Pts',(88.2469261659875,4.32873726556118,-0.958913468093504));
#11601=CARTESIAN_POINT('Ctrl Pts',(88.251907075901,4.35187709583085,-0.840660627934606));
#11602=CARTESIAN_POINT('Ctrl Pts',(88.2521787203491,4.35313907537538,-0.834211459396023));
#11603=CARTESIAN_POINT('Ctrl Pts',(88.2524496271672,4.35438579664064,-0.827759467187727));
#11604=CARTESIAN_POINT('Ctrl Pts',(88.2527197824194,4.35561720581304,-0.821304722628005));
#11605=CARTESIAN_POINT('Ctrl Pts',(88.2579490955998,4.37945321922404,-0.696362192282912));
#11606=CARTESIAN_POINT('Ctrl Pts',(88.2631187405,4.39792870993742,-0.570461397596616));
#11607=CARTESIAN_POINT('Ctrl Pts',(88.2682930712937,4.41095577524266,-0.444096649467237));
#11608=CARTESIAN_POINT('Ctrl Pts',(88.273470536565,4.42399073201151,-0.317655352799297));
#11609=CARTESIAN_POINT('Ctrl Pts',(88.278653056201,4.43157026328032,-0.190749581896201));
#11610=CARTESIAN_POINT('Ctrl Pts',(88.2839211452246,4.43364893135705,-0.0638892175160819));
#11611=CARTESIAN_POINT('Ctrl Pts',(88.2887880663573,4.43556930771089,0.0533106600021103));
#11612=CARTESIAN_POINT('Ctrl Pts',(88.2937284667628,4.43279464093632,0.170472300102315));
#11613=CARTESIAN_POINT('Ctrl Pts',(88.2988132543505,4.42532704257903,0.287181357734377));
#11614=CARTESIAN_POINT('Ctrl Pts',(88.299240263372,4.42469993047012,0.296982321813913));
#11615=CARTESIAN_POINT('Ctrl Pts',(88.2996682906498,4.42403973806537,0.306780120379378));
#11616=CARTESIAN_POINT('Ctrl Pts',(88.3000973781779,4.42334647486158,0.316574522647752));
#11617=CARTESIAN_POINT('Ctrl Pts',(88.3025226835781,4.41942798531884,0.371934828309909));
#11618=CARTESIAN_POINT('Ctrl Pts',(88.3049819359955,4.41445307170498,0.427185484136135));
#11619=CARTESIAN_POINT('Ctrl Pts',(88.3074828440316,4.40842550340863,0.482281762922626));
#11620=CARTESIAN_POINT('Ctrl Pts',(88.3074848791918,4.40842059836357,0.482326598537384));
#11621=CARTESIAN_POINT('Ctrl Pts',(88.3074869143795,4.40841569262152,0.482371434050032));
#11622=CARTESIAN_POINT('Ctrl Pts',(88.3074889495948,4.40841078618251,0.482416269460595));
#11623=CARTESIAN_POINT('Ctrl Pts',(88.3126742520122,4.39591020693204,0.596647507606413));
#11624=CARTESIAN_POINT('Ctrl Pts',(88.3180489665222,4.37884196458973,0.710528809899669));
#11625=CARTESIAN_POINT('Ctrl Pts',(88.3235362150093,4.35727595214971,0.823677263995305));
#11626=CARTESIAN_POINT('Ctrl Pts',(88.324093059376,4.35508743953416,0.835159535922351));
#11627=CARTESIAN_POINT('Ctrl Pts',(88.3246510626323,4.35285263999814,0.846634230001444));
#11628=CARTESIAN_POINT('Ctrl Pts',(88.3252101444366,4.35057164841986,0.858100925614195));
#11629=CARTESIAN_POINT('Ctrl Pts',(88.3312711206446,4.3258435396182,0.982410764987429));
#11630=CARTESIAN_POINT('Ctrl Pts',(88.3374583186823,4.29568264521297,1.1057850158928));
#11631=CARTESIAN_POINT('Ctrl Pts',(88.34368016388,4.26022787552279,1.2277347657466));
#11632=CARTESIAN_POINT('Ctrl Pts',(88.3498959671657,4.22480753526435,1.34956609258924));
#11633=CARTESIAN_POINT('Ctrl Pts',(88.3561459994899,4.18410394590584,1.46997581808843));
#11634=CARTESIAN_POINT('Ctrl Pts',(88.3623563326784,4.13829217149236,1.58849812001653));
#11635=CARTESIAN_POINT('Ctrl Pts',(88.3670758699542,4.10347755358855,1.67856903972076));
#11636=CARTESIAN_POINT('Ctrl Pts',(88.3717723604219,4.06571167236231,1.76755266132706));
#11637=CARTESIAN_POINT('Ctrl Pts',(88.376328904677,4.02494199509197,1.85517697637475));
#11638=CARTESIAN_POINT('Ctrl Pts',(88.3777638830742,4.01210252665498,1.88277223105159));
#11639=CARTESIAN_POINT('Ctrl Pts',(88.3791849817519,3.99896531190463,1.91023232068102));
#11640=CARTESIAN_POINT('Ctrl Pts',(88.3805885494597,3.9855292098289,1.93754780151039));
#11641=CARTESIAN_POINT('Ctrl Pts',(88.3854995300537,3.93851727290297,2.03312266798681));
#11642=CARTESIAN_POINT('Ctrl Pts',(88.3902867462941,3.88798972519749,2.12699235899576));
#11643=CARTESIAN_POINT('Ctrl Pts',(88.3950531015701,3.83427102944813,2.21900529470237));
#11644=CARTESIAN_POINT('Ctrl Pts',(88.395972404337,3.82391012624636,2.23675213510622));
#11645=CARTESIAN_POINT('Ctrl Pts',(88.3968909310737,3.81343042827611,2.25443003525906));
#11646=CARTESIAN_POINT('Ctrl Pts',(88.3978094201026,3.80283413819877,2.27203809196612));
#11647=CARTESIAN_POINT('Ctrl Pts',(88.4053579462217,3.71574940457759,2.41674844971666));
#11648=CARTESIAN_POINT('Ctrl Pts',(88.4129040072771,3.62079221164668,2.55674564623762));
#11649=CARTESIAN_POINT('Ctrl Pts',(88.4204529529702,3.5185357059676,2.69119109358107));
#11650=CARTESIAN_POINT('Ctrl Pts',(88.4242643804918,3.4669068725042,2.75907197377261));
#11651=CARTESIAN_POINT('Ctrl Pts',(88.428076527498,3.41341680396074,2.8255368598138));
#11652=CARTESIAN_POINT('Ctrl Pts',(88.4318900102808,3.35813659260551,2.89047338262495));
#11653=CARTESIAN_POINT('Ctrl Pts',(88.4375750651803,3.27572608905717,2.98727929946844));
#11654=CARTESIAN_POINT('Ctrl Pts',(88.4430790529799,3.18909069641634,3.08048460237573));
#11655=CARTESIAN_POINT('Ctrl Pts',(88.4483028396688,3.09842148560063,3.16950016809463));
#11656=CARTESIAN_POINT('Ctrl Pts',(88.4535321800864,3.00765587877515,3.25861037173157));
#11657=CARTESIAN_POINT('Ctrl Pts',(88.4587018647028,2.91312064720813,3.34379064768385));
#11658=CARTESIAN_POINT('Ctrl Pts',(88.4638762505298,2.81517843687189,3.42469376862551));
#11659=CARTESIAN_POINT('Ctrl Pts',(88.4690537706853,2.7171768990968,3.50564589576117));
#11660=CARTESIAN_POINT('Ctrl Pts',(88.4742363605741,2.61576406817588,3.58231533116556));
#11661=CARTESIAN_POINT('Ctrl Pts',(88.4795045372405,2.51133909339373,3.65438155550048));
#11662=CARTESIAN_POINT('Ctrl Pts',(88.484371474871,2.41486741609302,3.72095901508639));
#11663=CARTESIAN_POINT('Ctrl Pts',(88.4893119047049,2.3158244805113,3.78360797795596));
#11664=CARTESIAN_POINT('Ctrl Pts',(88.4943967323435,2.21455627826925,3.84210047577926));
#11665=CARTESIAN_POINT('Ctrl Pts',(88.494823817067,2.20605056180728,3.84701337628132));
#11666=CARTESIAN_POINT('Ctrl Pts',(88.4952519204668,2.19752913362981,3.85189698180434));
#11667=CARTESIAN_POINT('Ctrl Pts',(88.4956810845568,2.18899219116201,3.85675117223813));
#11668=CARTESIAN_POINT('Ctrl Pts',(88.4981059652812,2.1407564050935,3.8841785201655));
#11669=CARTESIAN_POINT('Ctrl Pts',(88.5005647830725,2.09202633885257,3.91066624584325));
#11670=CARTESIAN_POINT('Ctrl Pts',(88.5030652419166,2.04284128277649,3.93619269992195));
#11671=CARTESIAN_POINT('Ctrl Pts',(88.5030672774364,2.04280124326366,3.93621347994879));
#11672=CARTESIAN_POINT('Ctrl Pts',(88.5030693129837,2.04276120344924,3.93623425933878));
#11673=CARTESIAN_POINT('Ctrl Pts',(88.5030713485587,2.04272116333327,3.93625503809191));
#11674=CARTESIAN_POINT('Ctrl Pts',(88.5082566148495,1.94072606743195,3.98918522740411));
#11675=CARTESIAN_POINT('Ctrl Pts',(88.5136312927532,1.83648974135252,4.03812022670876));
#11676=CARTESIAN_POINT('Ctrl Pts',(88.519118503124,1.7303695935858,4.08290589957153));
#11677=CARTESIAN_POINT('Ctrl Pts',(88.5196753212208,1.71960098536341,4.08745055367526));
#11678=CARTESIAN_POINT('Ctrl Pts',(88.5202332980985,1.70881302213459,4.09195249017283));
#11679=CARTESIAN_POINT('Ctrl Pts',(88.5207923534241,1.69800610649153,4.09641155483363));
#11680=CARTESIAN_POINT('Ctrl Pts',(88.5268532637511,1.58084463135547,4.14475380257966));
#11681=CARTESIAN_POINT('Ctrl Pts',(88.5330403934088,1.46144966914817,4.18805624318386));
#11682=CARTESIAN_POINT('Ctrl Pts',(88.5392621675087,1.34030510213326,4.22616340826203));
#11683=CARTESIAN_POINT('Ctrl Pts',(88.5454778997516,1.21927817650744,4.26423356813276));
#11684=CARTESIAN_POINT('Ctrl Pts',(88.5517278583337,1.09650512442358,4.29711890313276));
#11685=CARTESIAN_POINT('Ctrl Pts',(88.5579381145954,0.972470658038841,4.32470683472953));
#11686=CARTESIAN_POINT('Ctrl Pts',(88.5626572782554,0.87821706821998,4.34567085920162));
#11687=CARTESIAN_POINT('Ctrl Pts',(88.5673533963492,0.78323215765188,4.3635764621201));
#11688=CARTESIAN_POINT('Ctrl Pts',(88.5719095600084,0.687713116578562,4.37822909513413));
#11689=CARTESIAN_POINT('Ctrl Pts',(88.5733448188024,0.657623208939517,4.38284489078186));
#11690=CARTESIAN_POINT('Ctrl Pts',(88.5747661893163,0.62748068168726,4.38713782493833));
#11691=CARTESIAN_POINT('Ctrl Pts',(88.5761700169476,0.597292765902473,4.39110170631488));
#11692=CARTESIAN_POINT('Ctrl Pts',(88.5810811532897,0.491683667606262,4.40496890870523));
#11693=CARTESIAN_POINT('Ctrl Pts',(88.585868537906,0.385544406328172,4.41496466401966));
#11694=CARTESIAN_POINT('Ctrl Pts',(88.5906350694113,0.279181058186347,4.42127495133937));
#11695=CARTESIAN_POINT('Ctrl Pts',(88.5915540734545,0.258673830472536,4.42249159693455));
#11696=CARTESIAN_POINT('Ctrl Pts',(88.5924723023208,0.238158117201613,4.42357124503042));
#11697=CARTESIAN_POINT('Ctrl Pts',(88.5933904934974,0.217635889383263,4.42451522648365));
#11698=CARTESIAN_POINT('Ctrl Pts',(88.6009389625034,0.0489222221519416,
4.4322757178973));
#11699=CARTESIAN_POINT('Ctrl Pts',(88.6084849660381,-0.120233894879764,
4.43087153852246));
#11700=CARTESIAN_POINT('Ctrl Pts',(88.6160338539244,-0.288816798694789,
4.42031473652558));
#11701=CARTESIAN_POINT('Ctrl Pts',(88.6198451026491,-0.373930180537376,
4.41498486558931));
#11702=CARTESIAN_POINT('Ctrl Pts',(88.6236570707348,-0.458897106836972,
4.40732116841263));
#11703=CARTESIAN_POINT('Ctrl Pts',(88.6274703744389,-0.543584661866787,
4.39732050911107));
#11704=CARTESIAN_POINT('Ctrl Pts',(88.6331553118013,-0.669838294695528,
4.38241135785432));
#11705=CARTESIAN_POINT('Ctrl Pts',(88.6386594526455,-0.795438008294129,
4.36199051247216));
#11706=CARTESIAN_POINT('Ctrl Pts',(88.6438830995456,-0.919787444953118,
4.3358893920313));
#11707=CARTESIAN_POINT('Ctrl Pts',(88.649112301792,-1.04426912718779,4.30976051305939));
#11708=CARTESIAN_POINT('Ctrl Pts',(88.6542818371798,-1.16757034109364,4.27831575586976));
#11709=CARTESIAN_POINT('Ctrl Pts',(88.659456061486,-1.28920107037514,4.24166440484217));
#11710=CARTESIAN_POINT('Ctrl Pts',(88.6646334208795,-1.41090549629898,4.20499084658517));
#11711=CARTESIAN_POINT('Ctrl Pts',(88.6698158376551,-1.53093722145745,4.16310403275407));
#11712=CARTESIAN_POINT('Ctrl Pts',(88.6750838287784,-1.64880821876827,4.11615843292719));
#11713=CARTESIAN_POINT('Ctrl Pts',(88.6799506632503,-1.75770335915673,4.07278773275157));
#11714=CARTESIAN_POINT('Ctrl Pts',(88.6848909813306,-1.86475477089872,4.02509910080773));
#11715=CARTESIAN_POINT('Ctrl Pts',(88.6899756930262,-1.969580903352,3.97325408725581));
#11716=CARTESIAN_POINT('Ctrl Pts',(88.6904026931122,-1.97838391328691,3.96890028578768));
#11717=CARTESIAN_POINT('Ctrl Pts',(88.6908307114877,-1.98717126031601,3.96451717697275));
#11718=CARTESIAN_POINT('Ctrl Pts',(88.6912597901471,-1.99594273513131,3.96010485846834));
#11719=CARTESIAN_POINT('Ctrl Pts',(88.6936858775379,-2.04553822066947,3.93515682142974));
#11720=CARTESIAN_POINT('Ctrl Pts',(88.6961459363321,-2.09462526231771,3.9092755064484));
#11721=CARTESIAN_POINT('Ctrl Pts',(88.6986476831803,-2.14316399688096,3.8824816417897));
#11722=CARTESIAN_POINT('Ctrl Pts',(88.6986497189937,-2.14320349560607,3.88245983810024));
#11723=CARTESIAN_POINT('Ctrl Pts',(88.6986517548349,-2.14324299396828,3.88243803380654));
#11724=CARTESIAN_POINT('Ctrl Pts',(88.6986537907036,-2.14328249196755,3.88241622890861));
#11725=CARTESIAN_POINT('Ctrl Pts',(88.7038390036501,-2.24388108934445,3.82688070335949));
#11726=CARTESIAN_POINT('Ctrl Pts',(88.7092136440908,-2.34239745323425,3.76726498132466));
#11727=CARTESIAN_POINT('Ctrl Pts',(88.7147008378216,-2.43850516198815,3.70378103859378));
#11728=CARTESIAN_POINT('Ctrl Pts',(88.715257811622,-2.44826050842178,3.69733714494214));
#11729=CARTESIAN_POINT('Ctrl Pts',(88.7158159450729,-2.45799102189141,3.69085343770561));
#11730=CARTESIAN_POINT('Ctrl Pts',(88.7163751577785,-2.46769635055009,3.68433016662363));
#11731=CARTESIAN_POINT('Ctrl Pts',(88.7224362182404,-2.57288813752917,3.61362730161045));
#11732=CARTESIAN_POINT('Ctrl Pts',(88.7286235276674,-2.67512390579113,3.53827128339158));
#11733=CARTESIAN_POINT('Ctrl Pts',(88.7348455065168,-2.7740059773852,3.4585786252878));
#11734=CARTESIAN_POINT('Ctrl Pts',(88.7410614424553,-2.87279201272477,3.37896336629461));
#11735=CARTESIAN_POINT('Ctrl Pts',(88.7473116295912,-2.96823112133555,3.29502015789511));
#11736=CARTESIAN_POINT('Ctrl Pts',(88.7535221324707,-3.05996086175842,3.20708998389174));
#11737=CARTESIAN_POINT('Ctrl Pts',(88.7582392319246,-3.12963288620504,3.14030386627584));
#11738=CARTESIAN_POINT('Ctrl Pts',(88.7629333181917,-3.19716706686283,3.07121555595729));
#11739=CARTESIAN_POINT('Ctrl Pts',(88.7674874312259,-3.26229226916579,2.99988097650433));
#11740=CARTESIAN_POINT('Ctrl Pts',(88.7689249016892,-3.28284853424279,2.97736476968212));
#11741=CARTESIAN_POINT('Ctrl Pts',(88.7703484266155,-3.30316453263051,2.95462505731032));
#11742=CARTESIAN_POINT('Ctrl Pts',(88.7717543279102,-3.32323105067908,2.9316644304787));
#11743=CARTESIAN_POINT('Ctrl Pts',(88.7766673796261,-3.39335534838363,2.85142640275877));
#11744=CARTESIAN_POINT('Ctrl Pts',(88.7814567905682,-3.46054933268302,2.76859868729222));
#11745=CARTESIAN_POINT('Ctrl Pts',(88.7862254087508,-3.52479785884816,2.68353934964454));
#11746=CARTESIAN_POINT('Ctrl Pts',(88.7871423864923,-3.53715247944622,2.66718293016405));
#11747=CARTESIAN_POINT('Ctrl Pts',(88.7880585953786,-3.5493982739841,2.65074386475562));
#11748=CARTESIAN_POINT('Ctrl Pts',(88.788974766708,-3.56153525544711,2.6342245144915));
#11749=CARTESIAN_POINT('Ctrl Pts',(88.7965234801215,-3.6615368510353,2.49811477505377));
#11750=CARTESIAN_POINT('Ctrl Pts',(88.8040697256586,-3.7541562003804,2.35655529785458));
#11751=CARTESIAN_POINT('Ctrl Pts',(88.8116188533203,-3.83884021040688,2.21039810832349));
#11752=CARTESIAN_POINT('Ctrl Pts',(88.8154300303283,-3.88159293183581,2.13661065297148));
#11753=CARTESIAN_POINT('Ctrl Pts',(88.8192419260727,-3.92232226499099,2.06165118863399));
#11754=CARTESIAN_POINT('Ctrl Pts',(88.8230551567911,-3.9609519189178,1.98562858541869));
#11755=CARTESIAN_POINT('Ctrl Pts',(88.828393156557,-4.01502813377317,1.87920737250479));
#11756=CARTESIAN_POINT('Ctrl Pts',(88.8335742164791,-4.06474427856229,1.77057398406374));
#11757=CARTESIAN_POINT('Ctrl Pts',(88.838511287705,-4.10970385415131,1.66005705526204));
#11758=CARTESIAN_POINT('Ctrl Pts',(88.8388322416987,-4.1126266305665,1.6528724617967));
#11759=CARTESIAN_POINT('Ctrl Pts',(88.8391521645551,-4.1155292997402,1.64567992572836));
#11760=CARTESIAN_POINT('Ctrl Pts',(88.8394710323585,-4.11841175074111,1.63847954472992));
#11761=CARTESIAN_POINT('Ctrl Pts',(88.8447004338847,-4.16568367190082,1.52039398394477));
#11762=CARTESIAN_POINT('Ctrl Pts',(88.8498701415704,-4.20787696739411,1.40034346845488));
#11763=CARTESIAN_POINT('Ctrl Pts',(88.8550445021581,-4.24481089794598,1.27879640065804));
#11764=CARTESIAN_POINT('Ctrl Pts',(88.8602219967361,-4.28176719852342,1.15717571461982));
#11765=CARTESIAN_POINT('Ctrl Pts',(88.8654045125985,-4.31345736365714,1.03405662772249));
#11766=CARTESIAN_POINT('Ctrl Pts',(88.870672558463,-4.33973936023666,0.909930938328787));
#11767=CARTESIAN_POINT('Ctrl Pts',(88.8755395577144,-4.36402055690264,0.795254708676689));
#11768=CARTESIAN_POINT('Ctrl Pts',(88.8804800061319,-4.38368570117873,0.679718783991746));
#11769=CARTESIAN_POINT('Ctrl Pts',(88.8855648133698,-4.39865768232481,0.563730302321979));
#11770=CARTESIAN_POINT('Ctrl Pts',(88.8859916895257,-4.39991459954097,0.553992919001472));
#11771=CARTESIAN_POINT('Ctrl Pts',(88.8864195830966,-4.40113846038811,0.544252323380795));
#11772=CARTESIAN_POINT('Ctrl Pts',(88.8868485360378,-4.40232923011608,0.534508743603727));
#11773=CARTESIAN_POINT('Ctrl Pts',(88.8892736617257,-4.4090613584635,0.47942250141758));
#11774=CARTESIAN_POINT('Ctrl Pts',(88.8917327225631,-4.41473568588615,0.424242022646549));
#11775=CARTESIAN_POINT('Ctrl Pts',(88.8942334257734,-4.41934736579121,0.36901192318767));
#11776=CARTESIAN_POINT('Ctrl Pts',(88.8942354594229,-4.41935111615261,0.368967008354615));
#11777=CARTESIAN_POINT('Ctrl Pts',(88.8942374931,-4.41935486581136,0.368922093488603));
#11778=CARTESIAN_POINT('Ctrl Pts',(88.8942395268047,-4.41935861476748,0.368877178589694));
#11779=CARTESIAN_POINT('Ctrl Pts',(88.8997640300927,-4.42954255200204,0.246867078456412));
#11780=CARTESIAN_POINT('Ctrl Pts',(88.9054973428673,-4.4345535582682,0.124431760651417));
#11781=CARTESIAN_POINT('Ctrl Pts',(88.9113509797045,-4.43441641653331,0.00189840082963779));
#11782=CARTESIAN_POINT('',(90.165602803248,-4.43009162062031,0.000681083854117898));
#11783=CARTESIAN_POINT('Ctrl Pts',(88.9113509797466,-4.43441641653234,0.00189839995022082));
#11784=CARTESIAN_POINT('Ctrl Pts',(88.9173338959108,-4.43427624595586,-0.123341145899187));
#11785=CARTESIAN_POINT('Ctrl Pts',(88.9234449643459,-4.42875229890772,-0.248759022069367));
#11786=CARTESIAN_POINT('Ctrl Pts',(88.9295950982453,-4.41787437557558,-0.373858329363207));
#11787=CARTESIAN_POINT('Ctrl Pts',(88.935738216371,-4.40700886124961,-0.498814929448322));
#11788=CARTESIAN_POINT('Ctrl Pts',(88.9419199606888,-4.39080193034475,-0.62345371073549));
#11789=CARTESIAN_POINT('Ctrl Pts',(88.9480676269832,-4.36932421936612,-0.747291815820922));
#11790=CARTESIAN_POINT('Ctrl Pts',(88.9528821545821,-4.35250401031208,-0.844275280142007));
#11791=CARTESIAN_POINT('Ctrl Pts',(88.9576756507821,-4.3324506045635,-0.940770445025382));
#11792=CARTESIAN_POINT('Ctrl Pts',(88.9623343406754,-4.30906855001,-1.03650676714499));
#11793=CARTESIAN_POINT('Ctrl Pts',(88.9636191068494,-4.30262028376824,-1.06290877953536));
#11794=CARTESIAN_POINT('Ctrl Pts',(88.9648936204995,-4.29591894294468,-1.08925278486935));
#11795=CARTESIAN_POINT('Ctrl Pts',(88.9661554953129,-4.28896273647101,-1.11553244321305));
#11796=CARTESIAN_POINT('Ctrl Pts',(88.9708462361282,-4.26310457583513,-1.21322126678081));
#11797=CARTESIAN_POINT('Ctrl Pts',(88.9754002049082,-4.23378922342771,-1.31003355369056));
#11798=CARTESIAN_POINT('Ctrl Pts',(88.9799269630748,-4.20130111295997,-1.40578832719475));
#11799=CARTESIAN_POINT('Ctrl Pts',(88.9810305276956,-4.19338093521012,-1.42913209251784));
#11800=CARTESIAN_POINT('Ctrl Pts',(88.982132475133,-4.18527211786431,-1.45241323844826));
#11801=CARTESIAN_POINT('Ctrl Pts',(88.9832343927969,-4.17697862060375,-1.47562958383669));
#11802=CARTESIAN_POINT('Ctrl Pts',(88.9910366261682,-4.11825572032538,-1.64001513702863));
#11803=CARTESIAN_POINT('Ctrl Pts',(88.9988374491339,-4.05027694435988,-1.80115607695242));
#11804=CARTESIAN_POINT('Ctrl Pts',(89.0066420079153,-3.97348734743145,-1.95800388872241));
#11805=CARTESIAN_POINT('Ctrl Pts',(89.0100812937322,-3.93964797495716,-2.02712303684359));
#11806=CARTESIAN_POINT('Ctrl Pts',(89.0135212944197,-3.90409705741618,-2.09540797673298));
#11807=CARTESIAN_POINT('Ctrl Pts',(89.0169624108972,-3.86687043079813,-2.16276657324726));
#11808=CARTESIAN_POINT('Ctrl Pts',(89.0209259000541,-3.82399268111743,-2.2403504239092));
#11809=CARTESIAN_POINT('Ctrl Pts',(89.024866759478,-3.77885276701861,-2.31668898180908));
#11810=CARTESIAN_POINT('Ctrl Pts',(89.0286617337184,-3.7313376756158,-2.39150141749011));
#11811=CARTESIAN_POINT('Ctrl Pts',(89.03025348207,-3.71140814154716,-2.42288043711618));
#11812=CARTESIAN_POINT('Ctrl Pts',(89.0318195653583,-3.69106108346295,-2.45399043620517));
#11813=CARTESIAN_POINT('Ctrl Pts',(89.03335088858,-3.67028971707157,-2.48480844640054));
#11814=CARTESIAN_POINT('Ctrl Pts',(89.0385383040655,-3.59992592571498,-2.5892056246388));
#11815=CARTESIAN_POINT('Ctrl Pts',(89.0436616318504,-3.52517434547603,-2.69057398178545));
#11816=CARTESIAN_POINT('Ctrl Pts',(89.0487810018849,-3.44631601856658,-2.78850971963755));
#11817=CARTESIAN_POINT('Ctrl Pts',(89.0539031865022,-3.3674143360712,-2.8864993016614));
#11818=CARTESIAN_POINT('Ctrl Pts',(89.0590217429199,-3.28440117759914,-2.98105218564797));
#11819=CARTESIAN_POINT('Ctrl Pts',(89.0642128413372,-3.19759783039276,-3.0717841564076));
#11820=CARTESIAN_POINT('Ctrl Pts',(89.0690717194451,-3.11634973037239,-3.15670945563363));
#11821=CARTESIAN_POINT('Ctrl Pts',(89.0739945734964,-3.03178069708182,-3.23828745757245));
#11822=CARTESIAN_POINT('Ctrl Pts',(89.0790519277941,-2.94418994334224,-3.31622257692865));
#11823=CARTESIAN_POINT('Ctrl Pts',(89.0794056240146,-2.9380641082281,-3.3216731258781));
#11824=CARTESIAN_POINT('Ctrl Pts',(89.0797599781006,-2.93192348817042,-3.32710587734651));
#11825=CARTESIAN_POINT('Ctrl Pts',(89.0801150141767,-2.92576818301997,-3.33252073945192));
#11826=CARTESIAN_POINT('Ctrl Pts',(89.0832867255829,-2.87077982306099,-3.38089435851757));
#11827=CARTESIAN_POINT('Ctrl Pts',(89.0865130198547,-2.81462079959568,-3.42783891667989));
#11828=CARTESIAN_POINT('Ctrl Pts',(89.0898115136332,-2.75737118641255,-3.47328798007162));
#11829=CARTESIAN_POINT('Ctrl Pts',(89.0898135509579,-2.75733582601542,-3.4733160518234));
#11830=CARTESIAN_POINT('Ctrl Pts',(89.0898155883101,-2.75730046520219,-3.47334412300495));
#11831=CARTESIAN_POINT('Ctrl Pts',(89.0898176256899,-2.75726510397288,-3.47337219361629));
#11832=CARTESIAN_POINT('Ctrl Pts',(89.0950027180926,-2.66727145434008,-3.54481136050984));
#11833=CARTESIAN_POINT('Ctrl Pts',(89.100377214712,-2.5743147573871,-3.61275793309621));
#11834=CARTESIAN_POINT('Ctrl Pts',(89.1058642294585,-2.47871632386883,-3.67699232012963));
#11835=CARTESIAN_POINT('Ctrl Pts',(89.1064208614938,-2.46901830899426,-3.68350859888005));
#11836=CARTESIAN_POINT('Ctrl Pts',(89.1069786514708,-2.45929315181934,-3.68998667577098));
#11837=CARTESIAN_POINT('Ctrl Pts',(89.1075375191209,-2.44954121765714,-3.69642632268717));
#11838=CARTESIAN_POINT('Ctrl Pts',(89.1135980364993,-2.34378851136875,-3.7662596580647));
#11839=CARTESIAN_POINT('Ctrl Pts',(89.1197847509611,-2.23488089520999,-3.83157395890725));
#11840=CARTESIAN_POINT('Ctrl Pts',(89.12600608789,-2.12326351852121,-3.89212417639549));
#11841=CARTESIAN_POINT('Ctrl Pts',(89.1322213835749,-2.01175452815221,-3.95261559645066));
#11842=CARTESIAN_POINT('Ctrl Pts',(89.1384708837593,-1.8975411877036,-4.00835252387812));
#11843=CARTESIAN_POINT('Ctrl Pts',(89.1446806593068,-1.78107766297801,-4.0591318470126));
#11844=CARTESIAN_POINT('Ctrl Pts',(89.1493984900141,-1.69259536776018,-4.09771105944098));
#11845=CARTESIAN_POINT('Ctrl Pts',(89.1540932717488,-1.60281148049522,-4.13342978859183));
#11846=CARTESIAN_POINT('Ctrl Pts',(89.158648061512,-1.51188218000379,-4.16605936590582));
#11847=CARTESIAN_POINT('Ctrl Pts',(89.1600841171735,-1.48321356003308,-4.17634697338509));
#11848=CARTESIAN_POINT('Ctrl Pts',(89.1615062570085,-1.454431448233,-4.18632737743233));
#11849=CARTESIAN_POINT('Ctrl Pts',(89.1629108159405,-1.42554176845313,-4.19599309903408));
#11850=CARTESIAN_POINT('Ctrl Pts',(89.1678221860351,-1.32452221984552,-4.22979156411283));
#11851=CARTESIAN_POINT('Ctrl Pts',(89.1726098369038,-1.22224222059819,-4.25989086882007));
#11852=CARTESIAN_POINT('Ctrl Pts',(89.1773766575176,-1.11903781963725,-4.28641505536395));
#11853=CARTESIAN_POINT('Ctrl Pts',(89.1782947088245,-1.09916148216865,-4.29152340033682));
#11854=CARTESIAN_POINT('Ctrl Pts',(89.1792119875025,-1.07925070535549,-4.29649917095072));
#11855=CARTESIAN_POINT('Ctrl Pts',(89.1801292285449,-1.05930767157052,-4.30134329367298));
#11856=CARTESIAN_POINT('Ctrl Pts',(89.1876773215829,-0.895193913554452,
-4.34120619481496));
#11857=CARTESIAN_POINT('Ctrl Pts',(89.1952229477402,-0.728894477958929,
-4.37215881116081));
#11858=CARTESIAN_POINT('Ctrl Pts',(89.2027714574259,-0.561408571912545,
-4.39401892309368));
#11859=CARTESIAN_POINT('Ctrl Pts',(89.2065817866909,-0.476865201647971,
-4.40505344880866));
#11860=CARTESIAN_POINT('Ctrl Pts',(89.2103928348589,-0.392019694905821,
-4.41377030824008));
#11861=CARTESIAN_POINT('Ctrl Pts',(89.2142052180091,-0.307001836397285,
-4.42014104547019));
#11862=CARTESIAN_POINT('Ctrl Pts',(89.2195926977515,-0.186858615635747,
-4.42914387032225));
#11863=CARTESIAN_POINT('Ctrl Pts',(89.2248182814199,-0.0663462498244123,
-4.43317662849193));
#11864=CARTESIAN_POINT('Ctrl Pts',(89.2297959854322,0.0540658861819156,
-4.43199935600868));
#11865=CARTESIAN_POINT('Ctrl Pts',(89.2300702234772,0.0606997858047717,
-4.43193449620516));
#11866=CARTESIAN_POINT('Ctrl Pts',(89.2303437091406,0.0673333681263032,
-4.43185382405887));
#11867=CARTESIAN_POINT('Ctrl Pts',(89.230616428044,0.0739665500860772,-4.43175730007139));
#11868=CARTESIAN_POINT('Ctrl Pts',(89.2358448414531,0.201134183399653,-4.429906796479));
#11869=CARTESIAN_POINT('Ctrl Pts',(89.2410135380339,0.328159136093043,-4.4226139610929));
#11870=CARTESIAN_POINT('Ctrl Pts',(89.2461868698266,0.454539645633857,-4.40989243909039));
#11871=CARTESIAN_POINT('Ctrl Pts',(89.2513633410308,0.580996848576844,-4.39716319709366));
#11872=CARTESIAN_POINT('Ctrl Pts',(89.2565448156254,0.706808705286119,-4.37899829750856));
#11873=CARTESIAN_POINT('Ctrl Pts',(89.2618118126829,0.831466778434383,-4.35545611086801));
#11874=CARTESIAN_POINT('Ctrl Pts',(89.2666780531963,0.946639838009085,-4.3337052078098));
#11875=CARTESIAN_POINT('Ctrl Pts',(89.2716177425898,1.06082850511061,-4.30736401137064));
#11876=CARTESIAN_POINT('Ctrl Pts',(89.2767018141772,1.17362740550761,-4.27651819701333));
#11877=CARTESIAN_POINT('Ctrl Pts',(89.2771284065388,1.18309209310655,-4.27392999805395));
#11878=CARTESIAN_POINT('Ctrl Pts',(89.2775560154217,1.1925470248249,-4.2713100942397));
#11879=CARTESIAN_POINT('Ctrl Pts',(89.2779846827297,1.20199197711683,-4.26865854129652));
#11880=CARTESIAN_POINT('Ctrl Pts',(89.2804174194646,1.25559317779004,-4.25361067053862));
#11881=CARTESIAN_POINT('Ctrl Pts',(89.2828843198736,1.30887186588578,-4.23754382354898));
#11882=CARTESIAN_POINT('Ctrl Pts',(89.2853931704633,1.36178458164836,-4.22047084351471));
#11883=CARTESIAN_POINT('Ctrl Pts',(89.2853952084884,1.36182756445652,-4.22045697454928));
#11884=CARTESIAN_POINT('Ctrl Pts',(89.2853972465412,1.36187054702332,-4.22044310492));
#11885=CARTESIAN_POINT('Ctrl Pts',(89.2853992846217,1.3619135293488,-4.22042923462687));
#11886=CARTESIAN_POINT('Ctrl Pts',(89.2905841332388,1.47125997204108,-4.18514340037289));
#11887=CARTESIAN_POINT('Ctrl Pts',(89.2959585034097,1.5793424061195,-4.14545545754308));
#11888=CARTESIAN_POINT('Ctrl Pts',(89.3014455490792,1.68580003074203,-4.10151105507363));
#11889=CARTESIAN_POINT('Ctrl Pts',(89.302003417907,1.69662359479236,-4.09704322051065));
#11890=CARTESIAN_POINT('Ctrl Pts',(89.3025624514413,1.70743033956042,-4.09253142511774));
#11891=CARTESIAN_POINT('Ctrl Pts',(89.3031225689211,1.7182198701591,-4.08797584763621));
#11892=CARTESIAN_POINT('Ctrl Pts',(89.3091844405166,1.83498956834246,-4.03867310895781));
#11893=CARTESIAN_POINT('Ctrl Pts',(89.3153727346175,1.94974656906805,-3.98423749500221));
#11894=CARTESIAN_POINT('Ctrl Pts',(89.3215958436397,2.06203998517011,-3.92490373965682));
#11895=CARTESIAN_POINT('Ctrl Pts',(89.3278129035323,2.17422424724299,-3.86562765927303));
#11896=CARTESIAN_POINT('Ctrl Pts',(89.3340643594162,2.28394991416172,-3.80146327097515));
#11897=CARTESIAN_POINT('Ctrl Pts',(89.3402762346915,2.39079602407734,-3.73267606524159));
#11898=CARTESIAN_POINT('Ctrl Pts',(89.3449806575245,2.47171350178485,-3.68058163530958));
#11899=CARTESIAN_POINT('Ctrl Pts',(89.3496622601,2.55098187085607,-3.62583411085816));
#11900=CARTESIAN_POINT('Ctrl Pts',(89.3542037665837,2.62832529390225,-3.56843478513252));
#11901=CARTESIAN_POINT('Ctrl Pts',(89.3556546766786,2.65303479364132,-3.55009697994909));
#11902=CARTESIAN_POINT('Ctrl Pts',(89.3570912877247,2.67754750425057,-3.53148875628806));
#11903=CARTESIAN_POINT('Ctrl Pts',(89.3585097756134,2.70185356454807,-3.5126108696137));
#11904=CARTESIAN_POINT('Ctrl Pts',(89.3634345461209,2.78624044571976,-3.4470697675156));
#11905=CARTESIAN_POINT('Ctrl Pts',(89.3682363559925,2.86823411515067,-3.37841200418008));
#11906=CARTESIAN_POINT('Ctrl Pts',(89.3730177436943,2.94774968628422,-3.30698727416143));
#11907=CARTESIAN_POINT('Ctrl Pts',(89.3739221568034,2.96279028315424,-3.29347708294421));
#11908=CARTESIAN_POINT('Ctrl Pts',(89.3748258392316,2.97774232400135,-3.27986778830696));
#11909=CARTESIAN_POINT('Ctrl Pts',(89.3757294849248,2.9926053801036,-3.26616160620787));
#11910=CARTESIAN_POINT('Ctrl Pts',(89.3832795785564,3.11678841562773,-3.15164442435767));
#11911=CARTESIAN_POINT('Ctrl Pts',(89.3908271894445,3.23476418346696,-3.03036523766907));
#11912=CARTESIAN_POINT('Ctrl Pts',(89.3983776688004,3.3458269082551,-2.90305519283047));
#11913=CARTESIAN_POINT('Ctrl Pts',(89.4021881937133,3.40187729389938,-2.83880521946445));
#11914=CARTESIAN_POINT('Ctrl Pts',(89.4059994334832,3.45616613254501,-2.77301887523525));
#11915=CARTESIAN_POINT('Ctrl Pts',(89.4098120041868,3.50859783251089,-2.70578840584286));
#11916=CARTESIAN_POINT('Ctrl Pts',(89.4148177941302,3.57743906767941,-2.61751683431374));
#11917=CARTESIAN_POINT('Ctrl Pts',(89.4196987459627,3.64290697351561,-2.52661684222504));
#11918=CARTESIAN_POINT('Ctrl Pts',(89.4243603851711,3.70459795403511,-2.43326738627589));
#11919=CARTESIAN_POINT('Ctrl Pts',(89.4249932219271,3.71297275917051,-2.42059481248169));
#11920=CARTESIAN_POINT('Ctrl Pts',(89.4256220169306,3.72127791977721,-2.40787716541439));
#11921=CARTESIAN_POINT('Ctrl Pts',(89.4262465338218,3.72951239114612,-2.39511495825405));
#11922=CARTESIAN_POINT('Ctrl Pts',(89.4314769467693,3.79847719621511,-2.28822975705153));
#11923=CARTESIAN_POINT('Ctrl Pts',(89.4366474907802,3.86283200099393,-2.17844509759039));
#11924=CARTESIAN_POINT('Ctrl Pts',(89.4418224571373,3.92230987519417,-2.06618623351969));
#11925=CARTESIAN_POINT('Ctrl Pts',(89.4470005519071,3.9818237054423,-1.95385950580816));
#11926=CARTESIAN_POINT('Ctrl Pts',(89.4521834368465,4.0364543234949,-1.83905547073047));
#11927=CARTESIAN_POINT('Ctrl Pts',(89.4574515713837,4.08596831636072,-1.7222297335028));
#11928=CARTESIAN_POINT('Ctrl Pts',(89.4623194214103,4.13172012656755,-1.61428067410462));
#11929=CARTESIAN_POINT('Ctrl Pts',(89.4672605040975,4.17310344574936,-1.50460496351978));
#11930=CARTESIAN_POINT('Ctrl Pts',(89.4723457326437,4.20996469303591,-1.39358768311256));
#11931=CARTESIAN_POINT('Ctrl Pts',(89.4727717610203,4.21305284083464,-1.38428691888595));
#11932=CARTESIAN_POINT('Ctrl Pts',(89.4731988011121,4.21610927368266,-1.37497672018469));
#11933=CARTESIAN_POINT('Ctrl Pts',(89.4736268946167,4.21913391429703,-1.36565730306687));
#11934=CARTESIAN_POINT('Ctrl Pts',(89.4760478287954,4.23623871911896,-1.31295457531239));
#11935=CARTESIAN_POINT('Ctrl Pts',(89.4785025261831,4.25232646398416,-1.25995813713637));
#11936=CARTESIAN_POINT('Ctrl Pts',(89.4809986540732,4.26738392615008,-1.20671064490624));
#11937=CARTESIAN_POINT('Ctrl Pts',(89.4810006752033,4.26739611826994,-1.20666753008381));
#11938=CARTESIAN_POINT('Ctrl Pts',(89.4810026963606,4.26740830971445,-1.20662441509673));
#11939=CARTESIAN_POINT('Ctrl Pts',(89.4810047175451,4.26742050048366,-1.20658129994494));
#11940=CARTESIAN_POINT('Ctrl Pts',(89.4861917547402,4.29870610289723,-1.0959333602064));
#11941=CARTESIAN_POINT('Ctrl Pts',(89.4915680031363,4.32562082854711,-0.983895404350818));
#11942=CARTESIAN_POINT('Ctrl Pts',(89.4970565467966,4.34808585448519,-0.870849151089466));
#11943=CARTESIAN_POINT('Ctrl Pts',(89.4976120258965,4.35035947261769,-0.859408077665633));
#11944=CARTESIAN_POINT('Ctrl Pts',(89.498168655221,4.35258753077173,-0.847956716715763));
#11945=CARTESIAN_POINT('Ctrl Pts',(89.4987263550352,4.35476995967272,-0.836495490889139));
#11946=CARTESIAN_POINT('Ctrl Pts',(89.5047871538682,4.37848749050107,-0.711940699322092));
#11947=CARTESIAN_POINT('Ctrl Pts',(89.5109738447826,4.3968140506005,-0.586215222197355));
#11948=CARTESIAN_POINT('Ctrl Pts',(89.5171949220758,4.4096950871461,-0.459824704450336));
#11949=CARTESIAN_POINT('Ctrl Pts',(89.5234099701794,4.42256363996781,-0.333556678734284));
#11950=CARTESIAN_POINT('Ctrl Pts',(89.5296589876668,4.42999759358508,-0.206624906597751));
#11951=CARTESIAN_POINT('Ctrl Pts',(89.5358681517012,4.43198454857099,-0.0795271829341869));
#11952=CARTESIAN_POINT('Ctrl Pts',(89.5406269195087,4.43350737150969,0.0178818325815445));
#11953=CARTESIAN_POINT('Ctrl Pts',(89.5453621565787,4.43183064963855,0.115391277068648));
#11954=CARTESIAN_POINT('Ctrl Pts',(89.5499579312158,4.42680655288177,0.212763109606407));
#11955=CARTESIAN_POINT('Ctrl Pts',(89.5513543258259,4.42528001553263,0.242348873240857));
#11956=CARTESIAN_POINT('Ctrl Pts',(89.5527378451727,4.42344446848295,0.271921568999827));
#11957=CARTESIAN_POINT('Ctrl Pts',(89.5541052372566,4.42129586055704,0.301473570175083));
#11958=CARTESIAN_POINT('Ctrl Pts',(89.5589866201823,4.41362565523155,0.406969744726389));
#11959=CARTESIAN_POINT('Ctrl Pts',(89.563742402052,4.40210444461492,0.512207558966018));
#11960=CARTESIAN_POINT('Ctrl Pts',(89.5684762919852,4.38697600267487,0.616929843529802));
#11961=CARTESIAN_POINT('Ctrl Pts',(89.5694306922429,4.38392595523184,0.638042918989072));
#11962=CARTESIAN_POINT('Ctrl Pts',(89.5703842026667,4.38072925578238,0.659135206687543));
#11963=CARTESIAN_POINT('Ctrl Pts',(89.5713376731298,4.37738784884745,0.680204850114617));
#11964=CARTESIAN_POINT('Ctrl Pts',(89.5788844684349,4.35094034454968,0.846972770317364));
#11965=CARTESIAN_POINT('Ctrl Pts',(89.5864288425466,4.31543097305138,1.01232512314864));
#11966=CARTESIAN_POINT('Ctrl Pts',(89.593976139271,4.27107536506261,1.17527016033225));
#11967=CARTESIAN_POINT('Ctrl Pts',(89.597793584079,4.24864016851367,1.2576882378122));
#11968=CARTESIAN_POINT('Ctrl Pts',(89.6016117602949,4.2239410393046,1.33948992067119));
#11969=CARTESIAN_POINT('Ctrl Pts',(89.60543128547,4.19700173026486,1.42054371498032));
#11970=CARTESIAN_POINT('Ctrl Pts',(89.6111185526549,4.15688914001854,1.54123269160687));
#11971=CARTESIAN_POINT('Ctrl Pts',(89.6165795575936,4.11143224684027,1.6601375750728));
#11972=CARTESIAN_POINT('Ctrl Pts',(89.6218045518171,4.06073151655111,1.77669543562417));
#11973=CARTESIAN_POINT('Ctrl Pts',(89.6270350820097,4.00997706798581,1.89337679118843));
#11974=CARTESIAN_POINT('Ctrl Pts',(89.6322066309984,3.95425048069523,2.0078268626318));
#11975=CARTESIAN_POINT('Ctrl Pts',(89.6373837123003,3.89375777934207,2.11958730871945));
#11976=CARTESIAN_POINT('Ctrl Pts',(89.6425639213951,3.83322853063225,2.23141527615749));
#11977=CARTESIAN_POINT('Ctrl Pts',(89.6477500340735,3.76792710080369,2.34055010825465));
#11978=CARTESIAN_POINT('Ctrl Pts',(89.6530226807491,3.69810344281083,2.4465445067072));
#11979=CARTESIAN_POINT('Ctrl Pts',(89.6578902916207,3.63364352018499,2.54439659465884));
#11980=CARTESIAN_POINT('Ctrl Pts',(89.6628320995932,3.56532911573377,2.63957259728861));
#11981=CARTESIAN_POINT('Ctrl Pts',(89.6679188913664,3.49339515664647,2.73173174790067));
#11982=CARTESIAN_POINT('Ctrl Pts',(89.6683500243098,3.48729836698028,2.73954273125576));
#11983=CARTESIAN_POINT('Ctrl Pts',(89.6687821987406,3.48117557438164,2.74733207408508));
#11984=CARTESIAN_POINT('Ctrl Pts',(89.6692154577563,3.47502692045516,2.75509958611351));
#11985=CARTESIAN_POINT('Ctrl Pts',(89.6716194560804,3.44091025305919,2.79819871440032));
#11986=CARTESIAN_POINT('Ctrl Pts',(89.6740569175401,3.40599811156927,2.84062486370988));
#11987=CARTESIAN_POINT('Ctrl Pts',(89.676535320568,3.3703179949989,2.88234419597204));
#11988=CARTESIAN_POINT('Ctrl Pts',(89.6765373770621,3.37028838885844,2.88237881324713));
#11989=CARTESIAN_POINT('Ctrl Pts',(89.6765394335843,3.37025878218922,2.88241343003576));
#11990=CARTESIAN_POINT('Ctrl Pts',(89.6765414901348,3.37022917499128,2.8824480463379));
#11991=CARTESIAN_POINT('Ctrl Pts',(89.6817246002952,3.29561035476463,2.96969127792232));
#11992=CARTESIAN_POINT('Ctrl Pts',(89.6870971351162,3.21742057117278,3.05407878664307));
#11993=CARTESIAN_POINT('Ctrl Pts',(89.6925821699911,3.13593264311377,3.13533383337643));
#11994=CARTESIAN_POINT('Ctrl Pts',(89.6931379074117,3.12767638003009,3.14356650119223));
#11995=CARTESIAN_POINT('Ctrl Pts',(89.6936947997026,3.11938630326912,3.15176700506032));
#11996=CARTESIAN_POINT('Ctrl Pts',(89.6942527668554,3.11106272600721,3.15993505256923));
#11997=CARTESIAN_POINT('Ctrl Pts',(89.7003103652556,3.02069739167921,3.24861187032716));
#11998=CARTESIAN_POINT('Ctrl Pts',(89.7064941172793,2.92637771691585,3.33346463487352));
#11999=CARTESIAN_POINT('Ctrl Pts',(89.7127124239763,2.82849292331517,3.41416809356799));
#12000=CARTESIAN_POINT('Ctrl Pts',(89.7189246893456,2.73070322861293,3.49479314570166));
#12001=CARTESIAN_POINT('Ctrl Pts',(89.72517109202,2.62935555257194,3.5712772566176));
#12002=CARTESIAN_POINT('Ctrl Pts',(89.7313776590001,2.52485602787657,3.64333458333348));
#12003=CARTESIAN_POINT('Ctrl Pts',(89.7360710253056,2.44583415480109,3.69782387352403));
#12004=CARTESIAN_POINT('Ctrl Pts',(89.7407414940435,2.36500744803604,3.7497834056166));
#12005=CARTESIAN_POINT('Ctrl Pts',(89.7452715010768,2.28248170464977,3.79895922126368));
#12006=CARTESIAN_POINT('Ctrl Pts',(89.7467277117614,2.25595307712563,3.8147672205978));
#12007=CARTESIAN_POINT('Ctrl Pts',(89.7481694077278,2.22924922615302,3.83028735963664));
#12008=CARTESIAN_POINT('Ctrl Pts',(89.7495926837077,2.2023746782247,3.84551066645313));
#12009=CARTESIAN_POINT('Ctrl Pts',(89.7545174974658,2.10938347676613,3.89818629079531));
#12010=CARTESIAN_POINT('Ctrl Pts',(89.7593195488321,2.01443638926538,3.94745303884877));
#12011=CARTESIAN_POINT('Ctrl Pts',(89.7641013390683,1.9178892102015,3.99336711653667));
#12012=CARTESIAN_POINT('Ctrl Pts',(89.764998372304,1.89977757749617,4.00198030357279));
#12013=CARTESIAN_POINT('Ctrl Pts',(89.765894692523,1.88160949962352,4.01047556339915));
#12014=CARTESIAN_POINT('Ctrl Pts',(89.7667909764052,1.86338713528538,4.01885334158174));
#12015=CARTESIAN_POINT('Ctrl Pts',(89.7743368307102,1.70997223056509,4.08938623280268));
#12016=CARTESIAN_POINT('Ctrl Pts',(89.7818801906671,1.55270916543701,4.15159685260309));
#12017=CARTESIAN_POINT('Ctrl Pts',(89.7894264133058,1.39254406239966,4.20511595881072));
#12018=CARTESIAN_POINT('Ctrl Pts',(89.7932274826785,1.31186811406322,4.23207379522788));
#12019=CARTESIAN_POINT('Ctrl Pts',(89.7970292629555,1.23045586309233,4.25682554070753));
#12020=CARTESIAN_POINT('Ctrl Pts',(89.800832368387,1.14842847364711,4.2793188753807));
#12021=CARTESIAN_POINT('Ctrl Pts',(89.805778431349,1.04174917166579,4.30857219257627));
#12022=CARTESIAN_POINT('Ctrl Pts',(89.810604176573,0.933969361096981,4.33380130625309));
#12023=CARTESIAN_POINT('Ctrl Pts',(89.8152137598078,0.825396603966911,4.35470532685636));
#12024=CARTESIAN_POINT('Ctrl Pts',(89.8158964139658,0.80931757028313,4.3578010983951));
#12025=CARTESIAN_POINT('Ctrl Pts',(89.8165743272599,0.793221238163659,4.36080200005832));
#12026=CARTESIAN_POINT('Ctrl Pts',(89.8172471883871,0.777108703461246,4.36370704470046));
#12027=CARTESIAN_POINT('Ctrl Pts',(89.8224691458586,0.65206214100666,4.3862525878435));
#12028=CARTESIAN_POINT('Ctrl Pts',(89.8276307488096,0.526115646042954,4.40343949263792));
#12029=CARTESIAN_POINT('Ctrl Pts',(89.8327962608015,0.399763398328317,4.41518556770788));
#12030=CARTESIAN_POINT('Ctrl Pts',(89.8379649469734,0.273333507817401,4.42693886067961));
#12031=CARTESIAN_POINT('Ctrl Pts',(89.8431379071372,0.146497411646854,4.4332442417418));
#12032=CARTESIAN_POINT('Ctrl Pts',(89.8483956324844,0.01976430259382,4.43406208281381));
#12033=CARTESIAN_POINT('Ctrl Pts',(89.8532570899878,-0.0974170987240542,
4.43481828427993));
#12034=CARTESIAN_POINT('Ctrl Pts',(89.8581914608689,-0.214510963110474,
4.43088287360859));
#12035=CARTESIAN_POINT('Ctrl Pts',(89.8632699008244,-0.331102946416727,
4.42226261826606));
#12036=CARTESIAN_POINT('Ctrl Pts',(89.8636918505398,-0.340790164263757,
4.42154639156649));
#12037=CARTESIAN_POINT('Ctrl Pts',(89.8641147948164,-0.350473943311404,
4.42079783849864));
#12038=CARTESIAN_POINT('Ctrl Pts',(89.8645387744674,-0.360154060141499,
4.42001697073321));
#12039=CARTESIAN_POINT('Ctrl Pts',(89.8670300356084,-0.417033438293562,
4.41542867147029));
#12040=CARTESIAN_POINT('Ctrl Pts',(89.8695571253028,-0.473785165872243,
4.40972479577506));
#12041=CARTESIAN_POINT('Ctrl Pts',(89.8721284688833,-0.530360614488174,
4.40291002433756));
#12042=CARTESIAN_POINT('Ctrl Pts',(89.8721305157863,-0.530405651043084,
4.40290459947862));
#12043=CARTESIAN_POINT('Ctrl Pts',(89.8721325627174,-0.530450687486401,
4.40289917391584));
#12044=CARTESIAN_POINT('Ctrl Pts',(89.8721346096765,-0.530495723818192,
4.40289374764922));
#12045=CARTESIAN_POINT('Ctrl Pts',(89.8773174883639,-0.644527236988256,
4.38915449827478));
#12046=CARTESIAN_POINT('Ctrl Pts',(89.8826906006202,-0.758158274707413,
4.37085577659649));
#12047=CARTESIAN_POINT('Ctrl Pts',(89.8881773330672,-0.871007550141101,
4.34807159512846));
#12048=CARTESIAN_POINT('Ctrl Pts',(89.8887424788253,-0.882631278824343,
4.34572477329344));
#12049=CARTESIAN_POINT('Ctrl Pts',(89.8893088300326,-0.894246682134268,
4.34333039628311));
#12050=CARTESIAN_POINT('Ctrl Pts',(89.8898763029661,-0.905853322338966,
4.34088856817269));
#12051=CARTESIAN_POINT('Ctrl Pts',(89.8959456543481,-1.02999100999629,4.31477223390734));
#12052=CARTESIAN_POINT('Ctrl Pts',(89.9021427817368,-1.15313066849812,4.28322378915472));
#12053=CARTESIAN_POINT('Ctrl Pts',(89.9083758714525,-1.27478404874763,4.24638798134476));
#12054=CARTESIAN_POINT('Ctrl Pts',(89.9146028639203,-1.39631842688783,4.20958820655599));
#12055=CARTESIAN_POINT('Ctrl Pts',(89.9208653940798,-1.51636957290059,4.16751175951246));
#12056=CARTESIAN_POINT('Ctrl Pts',(89.9270891863883,-1.63447285878813,4.12033933563166));
#12057=CARTESIAN_POINT('Ctrl Pts',(89.9317114380169,-1.72218515355638,4.08530558092051));
#12058=CARTESIAN_POINT('Ctrl Pts',(89.9363122075619,-1.80882584158771,4.04745984070014));
#12059=CARTESIAN_POINT('Ctrl Pts',(89.9407721234367,-1.89413224688722,4.00674055007368));
#12060=CARTESIAN_POINT('Ctrl Pts',(89.9423130277404,-1.92360567435756,3.99267200440341));
#12061=CARTESIAN_POINT('Ctrl Pts',(89.9438371182328,-1.95291941697748,3.9782606411765));
#12062=CARTESIAN_POINT('Ctrl Pts',(89.9453394717082,-1.98206136903127,3.96350461204857));
#12063=CARTESIAN_POINT('Ctrl Pts',(89.9503538005096,-2.07932698055376,3.91425416396182));
#12064=CARTESIAN_POINT('Ctrl Pts',(89.955250113313,-2.1747713328336,3.86135855748933));
#12065=CARTESIAN_POINT('Ctrl Pts',(89.9601286446972,-2.26823055634348,3.80515107825526));
#12066=CARTESIAN_POINT('Ctrl Pts',(89.9609401275364,-2.28377633233121,3.79580166523648));
#12067=CARTESIAN_POINT('Ctrl Pts',(89.9617511183963,-2.29926728034706,3.7863605533578));
#12068=CARTESIAN_POINT('Ctrl Pts',(89.962562078582,-2.31470275989553,3.77682919509475));
#12069=CARTESIAN_POINT('Ctrl Pts',(89.9701235366887,-2.45862441478185,3.68795804274576));
#12070=CARTESIAN_POINT('Ctrl Pts',(89.9776824090846,-2.59772786769584,3.59124350771912));
#12071=CARTESIAN_POINT('Ctrl Pts',(89.985244053236,-2.73117933405758,3.48727195385883));
#12072=CARTESIAN_POINT('Ctrl Pts',(89.9890536844359,-2.79841350426469,3.43489005548395));
#12073=CARTESIAN_POINT('Ctrl Pts',(89.9928640041446,-2.86421232880433,3.38066564527305));
#12074=CARTESIAN_POINT('Ctrl Pts',(89.9966756281,-2.92846479451651,3.32467103867188));
#12075=CARTESIAN_POINT('Ctrl Pts',(90.0006119242939,-2.99481885756006,3.26684493635301));
#12076=CARTESIAN_POINT('Ctrl Pts',(90.0045291630206,-3.05950369332435,3.20710090106199));
#12077=CARTESIAN_POINT('Ctrl Pts',(90.0083031414468,-3.12222395701885,3.14538182858948));
#12078=CARTESIAN_POINT('Ctrl Pts',(90.0099848246292,-3.15017207985835,3.11787983613289));
#12079=CARTESIAN_POINT('Ctrl Pts',(90.0116380621922,-3.17772961640656,3.08998615730642));
#12080=CARTESIAN_POINT('Ctrl Pts',(90.0132518649428,-3.20486813651541,3.06169815698806));
#12081=CARTESIAN_POINT('Ctrl Pts',(90.0184927423126,-3.29300137078605,2.96983194803096));
#12082=CARTESIAN_POINT('Ctrl Pts',(90.0236726666322,-3.37715683995339,2.87423383398628));
#12083=CARTESIAN_POINT('Ctrl Pts',(90.0288555389961,-3.45699080402158,2.77527061821678));
#12084=CARTESIAN_POINT('Ctrl Pts',(90.034041481007,-3.53687205115229,2.67624878975064));
#12085=CARTESIAN_POINT('Ctrl Pts',(90.0392307359719,-3.61242631811392,2.573857690922));
#12086=CARTESIAN_POINT('Ctrl Pts',(90.0445033950305,-3.68333694365767,2.46850028678336));
#12087=CARTESIAN_POINT('Ctrl Pts',(90.0493797745034,-3.74891810772849,2.37106127600172));
#12088=CARTESIAN_POINT('Ctrl Pts',(90.054327937649,-3.8105276228146,2.27108461766728));
#12089=CARTESIAN_POINT('Ctrl Pts',(90.0594187312763,-3.86794016046396,2.16892013463666));
#12090=CARTESIAN_POINT('Ctrl Pts',(90.0598401599257,-3.87269291415439,2.16046270279974));
#12091=CARTESIAN_POINT('Ctrl Pts',(90.0602625660136,-3.87741693269434,2.15199026474082));
#12092=CARTESIAN_POINT('Ctrl Pts',(90.0606859897318,-3.88211210247967,2.14350301148524));
#12093=CARTESIAN_POINT('Ctrl Pts',(90.0630498662488,-3.90832414758128,2.09612064294574));
#12094=CARTESIAN_POINT('Ctrl Pts',(90.0654455307188,-3.93363656390953,2.04827750127295));
#12095=CARTESIAN_POINT('Ctrl Pts',(90.0678800983053,-3.95802962213333,2.0000102121832));
#12096=CARTESIAN_POINT('Ctrl Pts',(90.0678820203875,-3.95804888036328,1.99997210533559));
#12097=CARTESIAN_POINT('Ctrl Pts',(90.0678839424939,-3.95806813802033,1.99993399822355));
#12098=CARTESIAN_POINT('Ctrl Pts',(90.0678858646246,-3.95808739510449,1.9998958908471));
#12099=CARTESIAN_POINT('Ctrl Pts',(90.0732309642032,-4.01163788139567,1.8939261332634));
#12100=CARTESIAN_POINT('Ctrl Pts',(90.0787724672161,-4.06087636930101,1.78565972066588));
#12101=CARTESIAN_POINT('Ctrl Pts',(90.0844273157989,-4.10565742180452,1.67547174493592));
#12102=CARTESIAN_POINT('Ctrl Pts',(90.0851576778716,-4.11144119865498,1.66124022004765));
#12103=CARTESIAN_POINT('Ctrl Pts',(90.0858899307157,-4.11715062444602,1.64697671170688));
#12104=CARTESIAN_POINT('Ctrl Pts',(90.0866238953809,-4.12278539225322,1.63268209105214));
#12105=CARTESIAN_POINT('Ctrl Pts',(90.0926958776793,-4.16940100197741,1.51442478562329));
#12106=CARTESIAN_POINT('Ctrl Pts',(90.0988843397485,-4.21090677877972,1.39403285447817));
#12107=CARTESIAN_POINT('Ctrl Pts',(90.1051009695411,-4.24716787846438,1.27196470229976));
#12108=CARTESIAN_POINT('Ctrl Pts',(90.1056667642231,-4.25046811316574,1.26085490267277));
#12109=CARTESIAN_POINT('Ctrl Pts',(90.1062327922292,-4.25372490028258,1.24973125374402));
#12110=CARTESIAN_POINT('Ctrl Pts',(90.1067989869812,-4.25693813637941,1.23859412245778));
#12111=CARTESIAN_POINT('Ctrl Pts',(90.1133457850976,-4.29409215088169,1.10981767253204));
#12112=CARTESIAN_POINT('Ctrl Pts',(90.1199146002839,-4.32542476178032,0.979232877876883));
#12113=CARTESIAN_POINT('Ctrl Pts',(90.1264255217307,-4.35081835891402,0.847375981929201));
#12114=CARTESIAN_POINT('Ctrl Pts',(90.1311208337292,-4.3691307993701,0.752288171287351));
#12115=CARTESIAN_POINT('Ctrl Pts',(90.1357859242796,-4.38435482539701,0.656535837450231));
#12116=CARTESIAN_POINT('Ctrl Pts',(90.1403067822695,-4.39629686998514,0.560308977345115));
#12117=CARTESIAN_POINT('Ctrl Pts',(90.1420457297909,-4.40089037610365,0.523295326341313));
#12118=CARTESIAN_POINT('Ctrl Pts',(90.1437633373064,-4.40499818958299,0.486212003666932));
#12119=CARTESIAN_POINT('Ctrl Pts',(90.1454531163204,-4.4086089998006,0.449071857940345));
#12120=CARTESIAN_POINT('Ctrl Pts',(90.1515246864034,-4.42158305564537,0.315623048476399));
#12121=CARTESIAN_POINT('Ctrl Pts',(90.1575222905921,-4.42863360464323,0.181494394818817));
#12122=CARTESIAN_POINT('Ctrl Pts',(90.1635243306403,-4.42988874177923,0.0471916357765029));
#12123=CARTESIAN_POINT('Ctrl Pts',(90.1642165712484,-4.43003350204195,0.0317019318033428));
#12124=CARTESIAN_POINT('Ctrl Pts',(90.1649088715641,-4.43010114383871,0.016209846318666));
#12125=CARTESIAN_POINT('Ctrl Pts',(90.1656012380541,-4.43009164223147,0.000716109671487679));
#12126=CARTESIAN_POINT('',(90.4404529603198,-0.735086155396302,-4.37342048255888));
#12127=CARTESIAN_POINT('Ctrl Pts',(90.165602803248,-4.43009162062031,0.000681083854117794));
#12128=CARTESIAN_POINT('Ctrl Pts',(90.1707097639098,-4.43002067830906,-0.113602183773604));
#12129=CARTESIAN_POINT('Ctrl Pts',(90.1758092756259,-4.42575708944723,-0.227727827826633));
#12130=CARTESIAN_POINT('Ctrl Pts',(90.1809092724363,-4.41731798229872,-0.34152341032841));
#12131=CARTESIAN_POINT('Ctrl Pts',(90.1817440651521,-4.41593662747877,-0.360150034402737));
#12132=CARTESIAN_POINT('Ctrl Pts',(90.182578870865,-4.41444328573784,-0.378767814898256));
#12133=CARTESIAN_POINT('Ctrl Pts',(90.1834137243702,-4.41283789931972,-0.39737599070201));
#12134=CARTESIAN_POINT('Ctrl Pts',(90.1873690216296,-4.40523203738054,-0.485536208395152));
#12135=CARTESIAN_POINT('Ctrl Pts',(90.1913231750305,-4.39511257454556,-0.573451544421442));
#12136=CARTESIAN_POINT('Ctrl Pts',(90.1951514067466,-4.38226713767787,-0.660932921087678));
#12137=CARTESIAN_POINT('Ctrl Pts',(90.1970739920729,-4.3758160003741,-0.704867150667409));
#12138=CARTESIAN_POINT('Ctrl Pts',(90.1989648177762,-4.36867737148063,-0.748691109347414));
#12139=CARTESIAN_POINT('Ctrl Pts',(90.2008080786697,-4.36082494922787,-0.792375921086213));
#12140=CARTESIAN_POINT('Ctrl Pts',(90.2063330165938,-4.33728832147512,-0.923315536818702));
#12141=CARTESIAN_POINT('Ctrl Pts',(90.2117707070029,-4.30791923130784,-1.05310610318921));
#12142=CARTESIAN_POINT('Ctrl Pts',(90.2171864362058,-4.27282885090481,-1.1812175042564));
#12143=CARTESIAN_POINT('Ctrl Pts',(90.222607978033,-4.2377008085011,-1.3094664054481));
#12144=CARTESIAN_POINT('Ctrl Pts',(90.2280078812813,-4.196838766294,-1.4360324910925));
#12145=CARTESIAN_POINT('Ctrl Pts',(90.2334727330767,-4.15039594311375,-1.56038459183445));
#12146=CARTESIAN_POINT('Ctrl Pts',(90.238510241917,-4.10758487684942,-1.67501255069715));
#12147=CARTESIAN_POINT('Ctrl Pts',(90.2436034111239,-4.06003122346315,-1.78775984788406));
#12148=CARTESIAN_POINT('Ctrl Pts',(90.2488311501934,-4.00789342145565,-1.89821015136766));
#12149=CARTESIAN_POINT('Ctrl Pts',(90.2492864425789,-4.00335265460874,-1.90782944978414));
#12150=CARTESIAN_POINT('Ctrl Pts',(90.2497427556707,-3.99877711660143,-1.91743135832675));
#12151=CARTESIAN_POINT('Ctrl Pts',(90.2502001415952,-3.99416691131452,-1.92701562069959));
#12152=CARTESIAN_POINT('Ctrl Pts',(90.2543767125297,-3.95206931195706,-2.01453329342759));
#12153=CARTESIAN_POINT('Ctrl Pts',(90.2586431109681,-3.90708214149884,-2.10057634447874));
#12154=CARTESIAN_POINT('Ctrl Pts',(90.2630407733878,-3.85930451175408,-2.1849389832888));
#12155=CARTESIAN_POINT('Ctrl Pts',(90.2630430193588,-3.85928011079705,-2.18498206891559));
#12156=CARTESIAN_POINT('Ctrl Pts',(90.263045265364,-3.85925570911223,-2.18502515410467));
#12157=CARTESIAN_POINT('Ctrl Pts',(90.2630475114035,-3.85923130669968,-2.18506823885598));
#12158=CARTESIAN_POINT('Ctrl Pts',(90.2681680836276,-3.80359812841056,-2.28329384034211));
#12159=CARTESIAN_POINT('Ctrl Pts',(90.2734765479204,-3.74402771634766,-2.37949948803224));
#12160=CARTESIAN_POINT('Ctrl Pts',(90.2788975726521,-3.68072380227128,-2.47336583383366));
#12161=CARTESIAN_POINT('Ctrl Pts',(90.2794264372809,-3.67454799554213,-2.48252325195699));
#12162=CARTESIAN_POINT('Ctrl Pts',(90.2799563732119,-3.66833669354543,-2.49165839202724));
#12163=CARTESIAN_POINT('Ctrl Pts',(90.2804873104987,-3.66209011058952,-2.50077094920276));
#12164=CARTESIAN_POINT('Ctrl Pts',(90.286453103996,-3.59190136154591,-2.6031627677783));
#12165=CARTESIAN_POINT('Ctrl Pts',(90.2925448128886,-3.51725277362374,-2.70270561453334));
#12166=CARTESIAN_POINT('Ctrl Pts',(90.2986730318616,-3.4384478477376,-2.79901488110601));
#12167=CARTESIAN_POINT('Ctrl Pts',(90.3047953212409,-3.35971917258546,-2.89523095994728));
#12168=CARTESIAN_POINT('Ctrl Pts',(90.3109537094259,-3.27684247910983,-2.98821992204621));
#12169=CARTESIAN_POINT('Ctrl Pts',(90.3170752134955,-3.19014680520275,-3.0776320499727));
#12170=CARTESIAN_POINT('Ctrl Pts',(90.3215723695297,-3.12645592652094,-3.14331856852439));
#12171=CARTESIAN_POINT('Ctrl Pts',(90.3260495078073,-3.06070174567111,-3.20707679023385));
#12172=CARTESIAN_POINT('Ctrl Pts',(90.330383628066,-2.99291157132991,-3.26864370849903));
#12173=CARTESIAN_POINT('Ctrl Pts',(90.3319451500303,-2.96848773445356,-3.29082539461065));
#12174=CARTESIAN_POINT('Ctrl Pts',(90.3334881074185,-2.94379998517365,-3.3127223158421));
#12175=CARTESIAN_POINT('Ctrl Pts',(90.3350067478521,-2.91885090253306,-3.33432114308619));
#12176=CARTESIAN_POINT('Ctrl Pts',(90.3399047748643,-2.83838334879142,-3.40398321511733));
#12177=CARTESIAN_POINT('Ctrl Pts',(90.3446814655348,-2.75535080696006,-3.47071309838439));
#12178=CARTESIAN_POINT('Ctrl Pts',(90.349439212882,-2.67011784007389,-3.53449765480226));
#12179=CARTESIAN_POINT('Ctrl Pts',(90.3502490910346,-2.6556092264956,-3.54535525503769));
#12180=CARTESIAN_POINT('Ctrl Pts',(90.3510584202878,-2.64103675453277,-3.55612758341785));
#12181=CARTESIAN_POINT('Ctrl Pts',(90.351867705681,-2.62640209807326,-3.5668146597885));
#12182=CARTESIAN_POINT('Ctrl Pts',(90.3597037234976,-2.48470001160771,-3.67029375573646));
#12183=CARTESIAN_POINT('Ctrl Pts',(90.3675357087112,-2.33716889767475,-3.76578490968642));
#12184=CARTESIAN_POINT('Ctrl Pts',(90.3753689217696,-2.18480170157244,-3.85268100517606));
#12185=CARTESIAN_POINT('Ctrl Pts',(90.3786586312147,-2.12081214832146,-3.88917470245394));
#12186=CARTESIAN_POINT('Ctrl Pts',(90.3819485489868,-2.0559694098737,-3.92415183380878));
#12187=CARTESIAN_POINT('Ctrl Pts',(90.3852390350962,-1.99034626550601,-3.95756476271203));
#12188=CARTESIAN_POINT('Ctrl Pts',(90.3892655267015,-1.910044744358,-3.99845138956899));
#12189=CARTESIAN_POINT('Ctrl Pts',(90.3932928919654,-1.82857022065426,-4.03699774700701));
#12190=CARTESIAN_POINT('Ctrl Pts',(90.397199183523,-1.74598958993834,-4.07291147552513));
#12191=CARTESIAN_POINT('Ctrl Pts',(90.3986951560361,-1.7143641078544,-4.08666517258424));
#12192=CARTESIAN_POINT('Ctrl Pts',(90.4001733716245,-1.68257689504952,-4.10003253309289));
#12193=CARTESIAN_POINT('Ctrl Pts',(90.401626980939,-1.6506335816544,-4.11299636490675));
#12194=CARTESIAN_POINT('Ctrl Pts',(90.4060004509793,-1.55452582923043,-4.15200060729765));
#12195=CARTESIAN_POINT('Ctrl Pts',(90.4102366354247,-1.45706409460434,-4.18748717072495));
#12196=CARTESIAN_POINT('Ctrl Pts',(90.4144432581645,-1.35857177087372,-4.2194740926336));
#12197=CARTESIAN_POINT('Ctrl Pts',(90.4152883106816,-1.33878602082146,-4.22589982428307));
#12198=CARTESIAN_POINT('Ctrl Pts',(90.4161321702282,-1.31895852969768,-4.23218440060831));
#12199=CARTESIAN_POINT('Ctrl Pts',(90.416975710102,-1.29909168785376,-4.238328071728));
#12200=CARTESIAN_POINT('Ctrl Pts',(90.4220255776036,-1.18015846121885,-4.27510727575999));
#12201=CARTESIAN_POINT('Ctrl Pts',(90.4270643029064,-1.05981722550044,-4.30683500699945));
#12202=CARTESIAN_POINT('Ctrl Pts',(90.4321674075888,-0.938541675499302,
-4.33338727789315));
#12203=CARTESIAN_POINT('Ctrl Pts',(90.4350118798256,-0.870942643839946,
-4.34818752246638));
#12204=CARTESIAN_POINT('Ctrl Pts',(90.4378766204331,-0.803053670559433,
-4.36138050238944));
#12205=CARTESIAN_POINT('Ctrl Pts',(90.4407762354097,-0.734959324739651,
-4.37295071025681));
#12206=CARTESIAN_POINT('',(90.4430005297901,-3.92880598357857,-2.05328335682078));
#12207=CARTESIAN_POINT('Origin',(90.4430005297901,0.,0.));
#12208=CARTESIAN_POINT('',(90.3466277144114,-4.43267344052904,-0.00114624657387179));
#12209=CARTESIAN_POINT('Ctrl Pts',(90.44300052979,-3.92880598357866,-2.05328335682061));
#12210=CARTESIAN_POINT('Ctrl Pts',(90.4401546791341,-3.95817780288558,-1.9970825508976));
#12211=CARTESIAN_POINT('Ctrl Pts',(90.4372863887623,-3.98633994636562,-1.94025870731795));
#12212=CARTESIAN_POINT('Ctrl Pts',(90.4289966894566,-4.06376532669901,-1.77522750359804));
#12213=CARTESIAN_POINT('Ctrl Pts',(90.4235406572539,-4.10990743027711,-1.66561748571758));
#12214=CARTESIAN_POINT('Ctrl Pts',(90.4101039791726,-4.21234597660604,-1.39199840839599));
#12215=CARTESIAN_POINT('Ctrl Pts',(90.4021252561662,-4.26353658600981,-1.22628504654762));
#12216=CARTESIAN_POINT('Ctrl Pts',(90.3864480400268,-4.34544435073715,-0.893010766269091));
#12217=CARTESIAN_POINT('Ctrl Pts',(90.3787599890444,-4.37647550152217,-0.725823258773799));
#12218=CARTESIAN_POINT('Ctrl Pts',(90.3628263225225,-4.42120597826071,-0.37281819892494));
#12219=CARTESIAN_POINT('Ctrl Pts',(90.3546129001533,-4.4329514196714,-0.187081780487825));
#12220=CARTESIAN_POINT('Ctrl Pts',(90.3464395730826,-4.432999849613,-0.00115469958862167));
#12221=CARTESIAN_POINT('',(89.0991895136418,-4.43415067741399,0.00275531766146416));
#12222=CARTESIAN_POINT('Ctrl Pts',(90.3466277144115,-4.43267344052904,-0.00114624657387175));
#12223=CARTESIAN_POINT('Ctrl Pts',(90.3459760545727,-4.43268280628598,0.0136036900692794));
#12224=CARTESIAN_POINT('Ctrl Pts',(90.3453245604975,-4.43261864583851,0.028354689417639));
#12225=CARTESIAN_POINT('Ctrl Pts',(90.3446731946637,-4.43248090953104,0.0431060695119233));
#12226=CARTESIAN_POINT('Ctrl Pts',(90.344672848187,-4.43248083626586,0.0431139161172652));
#12227=CARTESIAN_POINT('Ctrl Pts',(90.3446725017102,-4.43248076297986,0.0431217627225287));
#12228=CARTESIAN_POINT('Ctrl Pts',(90.3446721552336,-4.43248068967303,0.0431296093277615));
#12229=CARTESIAN_POINT('Ctrl Pts',(90.3389921652848,-4.43127892899438,0.171763487653303));
#12230=CARTESIAN_POINT('Ctrl Pts',(90.3333254577855,-4.42448064780808,0.300383748035732));
#12231=CARTESIAN_POINT('Ctrl Pts',(90.3276943091825,-4.41211904933905,0.428480496774987));
#12232=CARTESIAN_POINT('Ctrl Pts',(90.322063328146,-4.39975781871486,0.556573433731334));
#12233=CARTESIAN_POINT('Ctrl Pts',(90.3164678949856,-4.38183358365999,0.68414293178754));
#12234=CARTESIAN_POINT('Ctrl Pts',(90.3109043007945,-4.35841557100791,0.810682913480534));
#12235=CARTESIAN_POINT('Ctrl Pts',(90.3053380135185,-4.3349862227533,0.937284147464959));
#12236=CARTESIAN_POINT('Ctrl Pts',(90.2998034946352,-4.30605764424883,1.06285486888758));
#12237=CARTESIAN_POINT('Ctrl Pts',(90.294271839873,-4.27173637083049,1.18689170676658));
#12238=CARTESIAN_POINT('Ctrl Pts',(90.2887388252984,-4.237406660426,1.31095903585345));
#12239=CARTESIAN_POINT('Ctrl Pts',(90.2832084659097,-4.19768136407558,1.43349166454669));
#12240=CARTESIAN_POINT('Ctrl Pts',(90.2776289597445,-4.1527071038058,1.55398972719301));
#12241=CARTESIAN_POINT('Ctrl Pts',(90.2720441535644,-4.10769012214737,1.6746022518568));
#12242=CARTESIAN_POINT('Ctrl Pts',(90.266409763153,-4.05741385183719,1.79317617249455));
#12243=CARTESIAN_POINT('Ctrl Pts',(90.2606550472161,-4.00206984023319,1.9092157782696));
#12244=CARTESIAN_POINT('Ctrl Pts',(90.2569210652864,-3.96615954656902,1.98450877202425));
#12245=CARTESIAN_POINT('Ctrl Pts',(90.2531360399043,-3.92811657238451,2.05873488702302));
#12246=CARTESIAN_POINT('Ctrl Pts',(90.2492776676841,-3.88800440969381,2.1317606826182));
#12247=CARTESIAN_POINT('Ctrl Pts',(90.2492763279321,-3.88799048144944,2.13178603954383));
#12248=CARTESIAN_POINT('Ctrl Pts',(90.2492749881712,-3.88797655295561,2.13181139632481));
#12249=CARTESIAN_POINT('Ctrl Pts',(90.2492736484015,-3.88796262421228,2.13183675296122));
#12250=CARTESIAN_POINT('Ctrl Pts',(90.2437698354437,-3.83074294134805,2.23600255309212));
#12251=CARTESIAN_POINT('Ctrl Pts',(90.2381095631735,-3.76920679329261,2.33790767168564));
#12252=CARTESIAN_POINT('Ctrl Pts',(90.2323689587691,-3.70358949296031,2.4372061160339));
#12253=CARTESIAN_POINT('Ctrl Pts',(90.2319061972759,-3.69829995239287,2.4452107603427));
#12254=CARTESIAN_POINT('Ctrl Pts',(90.2314429137612,-3.69298391719379,2.45319845497206));
#12255=CARTESIAN_POINT('Ctrl Pts',(90.2309791481032,-3.68764152432475,2.46116901329943));
#12256=CARTESIAN_POINT('Ctrl Pts',(90.2247676729956,-3.6160878425176,2.56792319786844));
#12257=CARTESIAN_POINT('Ctrl Pts',(90.2184702026454,-3.53980092786857,2.67160582658075));
#12258=CARTESIAN_POINT('Ctrl Pts',(90.2121706056719,-3.45910916386875,2.77181810402713));
#12259=CARTESIAN_POINT('Ctrl Pts',(90.2079905892352,-3.40556718312877,2.83831267005192));
#12260=CARTESIAN_POINT('Ctrl Pts',(90.2038097784381,-3.3500840281035,2.90328168903946));
#12261=CARTESIAN_POINT('Ctrl Pts',(90.1997593752413,-3.29262497090729,2.96648169062228));
#12262=CARTESIAN_POINT('Ctrl Pts',(90.1977093955917,-3.26354394064544,2.99846831289321));
#12263=CARTESIAN_POINT('Ctrl Pts',(90.1956928204815,-3.2339573432479,3.03000119100896));
#12264=CARTESIAN_POINT('Ctrl Pts',(90.1937266595148,-3.20386440940588,3.06104529690031));
#12265=CARTESIAN_POINT('Ctrl Pts',(90.1876561158611,-3.11095214451587,3.15689431597545));
#12266=CARTESIAN_POINT('Ctrl Pts',(90.1816787366797,-3.01370303685225,3.24854285841778));
#12267=CARTESIAN_POINT('Ctrl Pts',(90.1757040350591,-2.9126910429949,3.33581269637835));
#12268=CARTESIAN_POINT('Ctrl Pts',(90.1681125337462,-2.78434443546821,3.44669841612231));
#12269=CARTESIAN_POINT('Ctrl Pts',(90.1605253070486,-2.6499183111191,3.55052330344395));
#12270=CARTESIAN_POINT('Ctrl Pts',(90.1529375359557,-2.51027349497431,3.64673662984613));
#12271=CARTESIAN_POINT('Ctrl Pts',(90.1455402580452,-2.37413450222593,3.74053449293175));
#12272=CARTESIAN_POINT('Ctrl Pts',(90.1381422793008,-2.23303135047545,3.82710087663271));
#12273=CARTESIAN_POINT('Ctrl Pts',(90.1307390996494,-2.08773673855552,3.90588875544471));
#12274=CARTESIAN_POINT('Ctrl Pts',(90.1284590629084,-2.04298879658348,3.93015390459643));
#12275=CARTESIAN_POINT('Ctrl Pts',(90.1261785467046,-1.99784343142811,3.95368080944968));
#12276=CARTESIAN_POINT('Ctrl Pts',(90.1238974385569,-1.95232333151512,3.97645254663137));
#12277=CARTESIAN_POINT('Ctrl Pts',(90.120288095957,-1.88029797141564,4.01248371909665));
#12278=CARTESIAN_POINT('Ctrl Pts',(90.116677252201,-1.80733007453952,4.04662617558732));
#12279=CARTESIAN_POINT('Ctrl Pts',(90.1132013108187,-1.73343462572613,4.0785860963781));
#12280=CARTESIAN_POINT('Ctrl Pts',(90.111124500852,-1.68928347709965,4.0976815513159));
#12281=CARTESIAN_POINT('Ctrl Pts',(90.1090958488609,-1.64480210839157,4.11599744313679));
#12282=CARTESIAN_POINT('Ctrl Pts',(90.1071444485185,-1.60000201691604,4.13346793574427));
#12283=CARTESIAN_POINT('Ctrl Pts',(90.1019203393616,-1.48006734076534,4.18023832848366));
#12284=CARTESIAN_POINT('Ctrl Pts',(90.0967384730707,-1.35817365721744,4.22177250611973));
#12285=CARTESIAN_POINT('Ctrl Pts',(90.0915271953053,-1.23480490907399,4.25789063602616));
#12286=CARTESIAN_POINT('Ctrl Pts',(90.0863120059555,-1.11134356036681,4.29403587619543));
#12287=CARTESIAN_POINT('Ctrl Pts',(90.0810669370124,-0.986404860549503,
4.32475649417719));
#12288=CARTESIAN_POINT('Ctrl Pts',(90.0757071653272,-0.86049691958104,4.34991189709947));
#12289=CARTESIAN_POINT('Ctrl Pts',(90.0708892919712,-0.74731886840151,4.37252396951906));
#12290=CARTESIAN_POINT('Ctrl Pts',(90.0659782570646,-0.633356997208761,
4.39063952015416));
#12291=CARTESIAN_POINT('Ctrl Pts',(90.0609079765421,-0.518999354946138,
4.40418981303012));
#12292=CARTESIAN_POINT('Ctrl Pts',(90.0603292350039,-0.50594612889639,4.40573649615903));
#12293=CARTESIAN_POINT('Ctrl Pts',(90.059748418682,-0.492887707095587,4.40722373908085));
#12294=CARTESIAN_POINT('Ctrl Pts',(90.0591654292988,-0.479824635580856,
4.40865146974588));
#12295=CARTESIAN_POINT('Ctrl Pts',(90.0577243294216,-0.44753384041861,4.41218069779911));
#12296=CARTESIAN_POINT('Ctrl Pts',(90.0562699471261,-0.415215046300762,
4.41534625760791));
#12297=CARTESIAN_POINT('Ctrl Pts',(90.0548008128143,-0.382877139566811,
4.41814722958272));
#12298=CARTESIAN_POINT('Ctrl Pts',(90.054798789602,-0.382832605550807,4.41815108692982));
#12299=CARTESIAN_POINT('Ctrl Pts',(90.0547967663617,-0.382788071498567,
4.41815494358551));
#12300=CARTESIAN_POINT('Ctrl Pts',(90.0547947430934,-0.382743537410013,
4.41815879954982));
#12301=CARTESIAN_POINT('Ctrl Pts',(90.0496438568243,-0.269367556159388,
4.42797540860405));
#12302=CARTESIAN_POINT('Ctrl Pts',(90.0443007339449,-0.155424616051288,
4.43333011903269));
#12303=CARTESIAN_POINT('Ctrl Pts',(90.0388435098811,-0.0412975804935338,
4.43421162112182));
#12304=CARTESIAN_POINT('Ctrl Pts',(90.0382961246298,-0.0298501018289632,
4.43430003992907));
#12305=CARTESIAN_POINT('Ctrl Pts',(90.0377475914027,-0.0184008069736915,
4.43434347760861));
#12306=CARTESIAN_POINT('Ctrl Pts',(90.0371979890515,-0.00695010601547379,
4.43434193920902));
#12307=CARTESIAN_POINT('Ctrl Pts',(90.0311772445115,0.118489214107905,4.43432508645914));
#12308=CARTESIAN_POINT('Ctrl Pts',(90.0250287201998,0.244102444284032,4.42890783060357));
#12309=CARTESIAN_POINT('Ctrl Pts',(90.0188450467448,0.369392047656091,4.41812376066608));
#12310=CARTESIAN_POINT('Ctrl Pts',(90.0126681507393,0.494544330717774,4.40735151031929));
#12311=CARTESIAN_POINT('Ctrl Pts',(90.006456522929,0.619373750359978,4.39122455526414));
#12312=CARTESIAN_POINT('Ctrl Pts',(90.000285056382,0.743397398104673,4.36981636870766));
#12313=CARTESIAN_POINT('Ctrl Pts',(89.9959935887821,0.82964002161633,4.35492970631035));
#12314=CARTESIAN_POINT('Ctrl Pts',(89.9917216379227,0.915496123635736,4.3374886777928));
#12315=CARTESIAN_POINT('Ctrl Pts',(89.9875975120029,1.00075473745206,4.31734639597503));
#12316=CARTESIAN_POINT('Ctrl Pts',(89.9857957713041,1.03800236699153,4.30854667219763));
#12317=CARTESIAN_POINT('Ctrl Pts',(89.9840222448516,1.0751353056168,4.29923153576687));
#12318=CARTESIAN_POINT('Ctrl Pts',(89.9822876314567,1.11213296432513,4.28938962248299));
#12319=CARTESIAN_POINT('Ctrl Pts',(89.9765854089283,1.23375596320608,4.25703614255743));
#12320=CARTESIAN_POINT('Ctrl Pts',(89.9709595043935,1.35406248890358,4.21956869603409));
#12321=CARTESIAN_POINT('Ctrl Pts',(89.9653350664398,1.47267873857721,4.17729808545643));
#12322=CARTESIAN_POINT('Ctrl Pts',(89.9578181933815,1.63120538582459,4.12080482934344));
#12323=CARTESIAN_POINT('Ctrl Pts',(89.9503038612709,1.78672211242187,4.05573225669743));
#12324=CARTESIAN_POINT('Ctrl Pts',(89.9427866730361,1.93829788308465,3.98247424239128));
#12325=CARTESIAN_POINT('Ctrl Pts',(89.9390572458216,2.01349765013797,3.9461294784061));
#12326=CARTESIAN_POINT('Ctrl Pts',(89.9353271292559,2.087726831229,3.90776935015616));
#12327=CARTESIAN_POINT('Ctrl Pts',(89.9315957262388,2.16086825554478,3.86743854561077));
#12328=CARTESIAN_POINT('Ctrl Pts',(89.9278649168943,2.23399804293748,3.8271141577639));
#12329=CARTESIAN_POINT('Ctrl Pts',(89.9241328014689,2.30604442307921,3.78481713282482));
#12330=CARTESIAN_POINT('Ctrl Pts',(89.9205306438533,2.376750530202,3.7404077105897));
#12331=CARTESIAN_POINT('Ctrl Pts',(89.9186992771012,2.41269810040138,3.71782959268345));
#12332=CARTESIAN_POINT('Ctrl Pts',(89.9169015017109,2.44829851603235,3.69470588076957));
#12333=CARTESIAN_POINT('Ctrl Pts',(89.9151545674447,2.48351371273066,3.67102106409027));
#12334=CARTESIAN_POINT('Ctrl Pts',(89.909966158297,2.58810313674178,3.60067696362935));
#12335=CARTESIAN_POINT('Ctrl Pts',(89.9048786606799,2.68962634065957,3.52588468656838));
#12336=CARTESIAN_POINT('Ctrl Pts',(89.8997947770881,2.78770740362052,3.44697707147542));
#12337=CARTESIAN_POINT('Ctrl Pts',(89.894707958871,2.88584508297904,3.36802390768252));
#12338=CARTESIAN_POINT('Ctrl Pts',(89.8896244151715,2.98053775781111,3.28494948472798));
#12339=CARTESIAN_POINT('Ctrl Pts',(89.8844647479072,3.07139943366342,3.19807491930894));
#12340=CARTESIAN_POINT('Ctrl Pts',(89.8796601096812,3.15600905260015,3.11717806366051));
#12341=CARTESIAN_POINT('Ctrl Pts',(89.8747890322157,3.23729699614213,3.03298564457149));
#12342=CARTESIAN_POINT('Ctrl Pts',(89.8697792690141,3.3149702118713,2.94579257164261));
#12343=CARTESIAN_POINT('Ctrl Pts',(89.8694011092043,3.32083334098665,2.93921084022147));
#12344=CARTESIAN_POINT('Ctrl Pts',(89.8690221591742,3.32667589746338,2.93261200491482));
#12345=CARTESIAN_POINT('Ctrl Pts',(89.8686423878504,3.33249776686566,2.92599618919944));
#12346=CARTESIAN_POINT('Ctrl Pts',(89.8656595065444,3.37822514098612,2.87403283182651));
#12347=CARTESIAN_POINT('Ctrl Pts',(89.8626258184445,3.4226750807397,2.82102318451257));
#12348=CARTESIAN_POINT('Ctrl Pts',(89.8595259106998,3.46579114681716,2.76703463778351));
#12349=CARTESIAN_POINT('Ctrl Pts',(89.8595237212501,3.46582159948368,2.76699650593709));
#12350=CARTESIAN_POINT('Ctrl Pts',(89.8595215317674,3.46585205148511,2.76695837360231));
#12351=CARTESIAN_POINT('Ctrl Pts',(89.8595193422516,3.46588250282147,2.76692024077916));
#12352=CARTESIAN_POINT('Ctrl Pts',(89.8543692890127,3.53750838798797,2.67722640338861));
#12353=CARTESIAN_POINT('Ctrl Pts',(89.8490257750254,3.60565138707983,2.58456934156202));
#12354=CARTESIAN_POINT('Ctrl Pts',(89.8435650967696,3.67009301325766,2.48926904948137));
#12355=CARTESIAN_POINT('Ctrl Pts',(89.8429876971703,3.67690692306713,2.47919221508768));
#12356=CARTESIAN_POINT('Ctrl Pts',(89.8424089876202,3.68367945113089,2.46908587614747));
#12357=CARTESIAN_POINT('Ctrl Pts',(89.8418290583168,3.69041034074978,2.45895044489462));
#12358=CARTESIAN_POINT('Ctrl Pts',(89.8357717864202,3.76071344199256,2.35308743274409));
#12359=CARTESIAN_POINT('Ctrl Pts',(89.8295819965756,3.82647422612893,2.2440445425874));
#12360=CARTESIAN_POINT('Ctrl Pts',(89.8233520562633,3.88744639021242,2.1322702560433));
#12361=CARTESIAN_POINT('Ctrl Pts',(89.8171280486777,3.94836049094936,2.02060241133594));
#12362=CARTESIAN_POINT('Ctrl Pts',(89.8108643291039,4.00449544456473,1.90620852481146));
#12363=CARTESIAN_POINT('Ctrl Pts',(89.8046358010831,4.05564734243885,1.78954584458124));
#12364=CARTESIAN_POINT('Ctrl Pts',(89.7986575819535,4.10474357406174,1.67757154434262));
#12365=CARTESIAN_POINT('Ctrl Pts',(89.7927121698193,4.14924971933642,1.56350533409205));
#12366=CARTESIAN_POINT('Ctrl Pts',(89.7868942478997,4.18893902239296,1.44773755178359));
#12367=CARTESIAN_POINT('Ctrl Pts',(89.786341412979,4.19271040898246,1.43673697913376));
#12368=CARTESIAN_POINT('Ctrl Pts',(89.7857897292086,4.19643829007812,1.42572107921797));
#12369=CARTESIAN_POINT('Ctrl Pts',(89.7852392778258,4.20012246378047,1.41469021034695));
#12370=CARTESIAN_POINT('Ctrl Pts',(89.7809239099003,4.22900524166714,1.32821162349435));
#12371=CARTESIAN_POINT('Ctrl Pts',(89.7767787296868,4.25504566299023,1.24076433038674));
#12372=CARTESIAN_POINT('Ctrl Pts',(89.7726824676602,4.27841042913659,1.15260502021653));
#12373=CARTESIAN_POINT('Ctrl Pts',(89.7710559962329,4.28768769809445,1.11760027732866));
#12374=CARTESIAN_POINT('Ctrl Pts',(89.7694372371741,4.29654329660154,1.08248272629045));
#12375=CARTESIAN_POINT('Ctrl Pts',(89.76781859898,4.30498822491254,1.04726622783332));
#12376=CARTESIAN_POINT('Ctrl Pts',(89.762124261694,4.33469731638056,0.923375279880136));
#12377=CARTESIAN_POINT('Ctrl Pts',(89.7564313736596,4.35932573440998,0.798257745962767));
#12378=CARTESIAN_POINT('Ctrl Pts',(89.7507376434564,4.37879903795454,0.67234307589075));
#12379=CARTESIAN_POINT('Ctrl Pts',(89.745043485553,4.39827380428987,0.546418947391886));
#12380=CARTESIAN_POINT('Ctrl Pts',(89.7393484389035,4.41259273882384,0.419696198040109));
#12381=CARTESIAN_POINT('Ctrl Pts',(89.7336518270546,4.42166204872297,0.292608380861909));
#12382=CARTESIAN_POINT('Ctrl Pts',(89.7295357695024,4.42821503188084,0.200781733101244));
#12383=CARTESIAN_POINT('Ctrl Pts',(89.7256197692987,4.43167936859243,0.10874537863679));
#12384=CARTESIAN_POINT('Ctrl Pts',(89.7217806440399,4.43222774455031,0.01672425278658));
#12385=CARTESIAN_POINT('Ctrl Pts',(89.7203048537282,4.43243854463399,-0.0186494005462728));
#12386=CARTESIAN_POINT('Ctrl Pts',(89.7188404231871,4.43221850992994,-0.0540213489622811));
#12387=CARTESIAN_POINT('Ctrl Pts',(89.7173803551925,4.43157755931919,-0.0893808614021613));
#12388=CARTESIAN_POINT('Ctrl Pts',(89.7121165382498,4.4292668130411,-0.216858486659978));
#12389=CARTESIAN_POINT('Ctrl Pts',(89.706909188104,4.42148516166803,-0.344173750615162));
#12390=CARTESIAN_POINT('Ctrl Pts',(89.7016933708314,4.40824775351063,-0.47082209257879));
#12391=CARTESIAN_POINT('Ctrl Pts',(89.6964743766283,4.39500228250815,-0.597547575471347));
#12392=CARTESIAN_POINT('Ctrl Pts',(89.6912465347313,4.37629401782769,-0.723605202379522));
#12393=CARTESIAN_POINT('Ctrl Pts',(89.6859288490779,4.35218306602042,-0.848483653270712));
#12394=CARTESIAN_POINT('Ctrl Pts',(89.6810303022826,4.3299725343339,-0.963519211080887));
#12395=CARTESIAN_POINT('Ctrl Pts',(89.6760550647583,4.30317726307267,-1.07755466769261));
#12396=CARTESIAN_POINT('Ctrl Pts',(89.6709326451315,4.27188377187853,-1.19018586613403));
#12397=CARTESIAN_POINT('Ctrl Pts',(89.6704866500888,4.26915913333694,-1.19999235599975));
#12398=CARTESIAN_POINT('Ctrl Pts',(89.6700395393016,4.26640040577432,-1.20978823152006));
#12399=CARTESIAN_POINT('Ctrl Pts',(89.6695912662433,4.2636076520595,-1.21957324377747));
#12400=CARTESIAN_POINT('Ctrl Pts',(89.6675923262973,4.25115420017972,-1.26320658625381));
#12401=CARTESIAN_POINT('Ctrl Pts',(89.6655702300742,4.23802442648274,-1.30662318331853));
#12402=CARTESIAN_POINT('Ctrl Pts',(89.6635207911676,4.22422522690175,-1.34979954849863));
#12403=CARTESIAN_POINT('Ctrl Pts',(89.6635188497135,4.22421215478146,-1.34984044990279));
#12404=CARTESIAN_POINT('Ctrl Pts',(89.6635169082349,4.22419908206048,-1.34988135109147));
#12405=CARTESIAN_POINT('Ctrl Pts',(89.6635149667318,4.22418600873881,-1.34992225206465));
#12406=CARTESIAN_POINT('Ctrl Pts',(89.6583048644347,4.18910322043729,-1.45968167056365));
#12407=CARTESIAN_POINT('Ctrl Pts',(89.6529079930652,4.14959267157002,-1.56817878203137));
#12408=CARTESIAN_POINT('Ctrl Pts',(89.6474012560416,4.1058005181601,-1.67505030023803));
#12409=CARTESIAN_POINT('Ctrl Pts',(89.6468528707784,4.1014395015599,-1.685693039375));
#12410=CARTESIAN_POINT('Ctrl Pts',(89.6463033959711,4.097036059829,-1.69631963423943));
#12411=CARTESIAN_POINT('Ctrl Pts',(89.6457529075683,4.0925903612991,-1.70692971118167));
#12412=CARTESIAN_POINT('Ctrl Pts',(89.6396818443409,4.04356095990179,-1.82394298092083));
#12413=CARTESIAN_POINT('Ctrl Pts',(89.6334880310768,3.98938717627061,-1.93895075589036));
#12414=CARTESIAN_POINT('Ctrl Pts',(89.6272624154904,3.93030319386788,-2.05150138426143));
#12415=CARTESIAN_POINT('Ctrl Pts',(89.6210427178731,3.87127537573925,-2.16394502383309));
#12416=CARTESIAN_POINT('Ctrl Pts',(89.6147916260043,3.8073470026313,-2.27393638612393));
#12417=CARTESIAN_POINT('Ctrl Pts',(89.6085823649858,3.73878303508661,-2.38105355206892));
#12418=CARTESIAN_POINT('Ctrl Pts',(89.6041348249192,3.6896723612287,-2.45777892823504));
#12419=CARTESIAN_POINT('Ctrl Pts',(89.5997088512995,3.63818159748146,-2.5330322726376));
#12420=CARTESIAN_POINT('Ctrl Pts',(89.5954279326346,3.58427791445395,-2.60655391409357));
#12421=CARTESIAN_POINT('Ctrl Pts',(89.5937364158637,3.56297898518335,-2.63560447526638));
#12422=CARTESIAN_POINT('Ctrl Pts',(89.5920675461215,3.5413036738783,-2.66438421010478));
#12423=CARTESIAN_POINT('Ctrl Pts',(89.5904289414706,3.51925137591093,-2.6928753608655));
#12424=CARTESIAN_POINT('Ctrl Pts',(89.5846453544389,3.44141601490496,-2.79343717116831));
#12425=CARTESIAN_POINT('Ctrl Pts',(89.5789579691856,3.35927397910321,-2.89069572507703));
#12426=CARTESIAN_POINT('Ctrl Pts',(89.5732719335314,3.27329233069242,-2.98443916131024));
#12427=CARTESIAN_POINT('Ctrl Pts',(89.5657253493348,3.15917631233561,-3.1088567304979));
#12428=CARTESIAN_POINT('Ctrl Pts',(89.5581810590132,3.03829189927785,-3.22709219992152));
#12429=CARTESIAN_POINT('Ctrl Pts',(89.5506337359625,2.91136391121407,-3.33843728344095));
#12430=CARTESIAN_POINT('Ctrl Pts',(89.5468091382022,2.84704329109342,-3.39486128360517));
#12431=CARTESIAN_POINT('Ctrl Pts',(89.5429837790236,2.78117040080886,-3.44951501313159));
#12432=CARTESIAN_POINT('Ctrl Pts',(89.5391570428513,2.71383792200217,-3.50230130715213));
#12433=CARTESIAN_POINT('Ctrl Pts',(89.5342574925378,2.62762898237659,-3.56988608221051));
#12434=CARTESIAN_POINT('Ctrl Pts',(89.5294761247725,2.53889519243924,-3.63424724803423));
#12435=CARTESIAN_POINT('Ctrl Pts',(89.5249098565493,2.44779504547448,-3.69499323623541));
#12436=CARTESIAN_POINT('Ctrl Pts',(89.5241721915046,2.43307812769937,-3.70480654327509));
#12437=CARTESIAN_POINT('Ctrl Pts',(89.5234401399771,2.41829955003909,-3.71452544867758));
#12438=CARTESIAN_POINT('Ctrl Pts',(89.522714110562,2.40346009316782,-3.72414824077537));
#12439=CARTESIAN_POINT('Ctrl Pts',(89.5174882232391,2.2966471625415,-3.79341213861807));
#12440=CARTESIAN_POINT('Ctrl Pts',(89.5123205431825,2.18691980194012,-3.85806396624029));
#12441=CARTESIAN_POINT('Ctrl Pts',(89.5071461802061,2.07470347374617,-3.91783526245825));
#12442=CARTESIAN_POINT('Ctrl Pts',(89.5019686383418,1.96241820505896,-3.97764327938085));
#12443=CARTESIAN_POINT('Ctrl Pts',(89.4967840377611,1.84764079703562,-4.03256437854672));
#12444=CARTESIAN_POINT('Ctrl Pts',(89.4915114992318,1.73082731385916,-4.0823636412585));
#12445=CARTESIAN_POINT('Ctrl Pts',(89.4866513945994,1.62315133433679,-4.12826745515198));
#12446=CARTESIAN_POINT('Ctrl Pts',(89.4817161226339,1.51374484382532,-4.16981953397608));
#12447=CARTESIAN_POINT('Ctrl Pts',(89.4766351649714,1.40299072259745,-4.20686624248983));
#12448=CARTESIAN_POINT('Ctrl Pts',(89.4761960741052,1.3934194712202,-4.21006777897402));
#12449=CARTESIAN_POINT('Ctrl Pts',(89.4757558952248,1.38383813607468,-4.21323569409507));
#12450=CARTESIAN_POINT('Ctrl Pts',(89.4753145828178,1.37424695298452,-4.21636990312836));
#12451=CARTESIAN_POINT('Ctrl Pts',(89.4729470438029,1.32279247355333,-4.23318420984324));
#12452=CARTESIAN_POINT('Ctrl Pts',(89.4705468144635,1.2710556184954,-4.24902812032458));
#12453=CARTESIAN_POINT('Ctrl Pts',(89.4681067685567,1.21907612530969,-4.26388921464172));
#12454=CARTESIAN_POINT('Ctrl Pts',(89.4681047207161,1.21903250083773,-4.2639016870102));
#12455=CARTESIAN_POINT('Ctrl Pts',(89.4681026728475,1.21898887619474,-4.26391415868658));
#12456=CARTESIAN_POINT('Ctrl Pts',(89.4681006249508,1.21894525138081,-4.26392662967084));
#12457=CARTESIAN_POINT('Ctrl Pts',(89.4629203670265,1.1085940830698,-4.29547261369915));
#12458=CARTESIAN_POINT('Ctrl Pts',(89.4575502385208,0.99684079441647,-4.32266856133506));
#12459=CARTESIAN_POINT('Ctrl Pts',(89.4520672413171,0.884065361812501,-4.34543406395382));
#12460=CARTESIAN_POINT('Ctrl Pts',(89.4515107322709,0.872618967423584,-4.34774469948338));
#12461=CARTESIAN_POINT('Ctrl Pts',(89.4509530604866,0.8611620838353,-4.35000971158681));
#12462=CARTESIAN_POINT('Ctrl Pts',(89.4503943064768,0.849695135570088,-4.35222902864808));
#12463=CARTESIAN_POINT('Ctrl Pts',(89.4443379353231,0.72540413546552,-4.37628435101583));
#12464=CARTESIAN_POINT('Ctrl Pts',(89.4381549530938,0.599925051924999,-4.39496914330591));
#12465=CARTESIAN_POINT('Ctrl Pts',(89.4319370866374,0.473761887533089,-4.40822664556218));
#12466=CARTESIAN_POINT('Ctrl Pts',(89.4257253525158,0.347723150833167,-4.42147107268344));
#12467=CARTESIAN_POINT('Ctrl Pts',(89.4194791529364,0.221001690369546,-4.42929928245315));
#12468=CARTESIAN_POINT('Ctrl Pts',(89.4132725672592,0.0940938886779707,
-4.4316966952617));
#12469=CARTESIAN_POINT('Ctrl Pts',(89.4085779942434,-0.00189736517690565,
-4.43351006416758));
#12470=CARTESIAN_POINT('Ctrl Pts',(89.4039062033646,-0.0979982089428208,
-4.43221631699086));
#12471=CARTESIAN_POINT('Ctrl Pts',(89.3993747311469,-0.193980083124144,
-4.42766206395347));
#12472=CARTESIAN_POINT('Ctrl Pts',(89.3979196587155,-0.224800216698573,
-4.42619967651687));
#12473=CARTESIAN_POINT('Ctrl Pts',(89.3964790542012,-0.255607682421183,
-4.42440112899348));
#12474=CARTESIAN_POINT('Ctrl Pts',(89.3950568090295,-0.286393777394904,
-4.42226145416874));
#12475=CARTESIAN_POINT('Ctrl Pts',(89.3901348141735,-0.392935887093349,
-4.41485663487967));
#12476=CARTESIAN_POINT('Ctrl Pts',(89.3853357505001,-0.49922878422454,-4.40353431601429));
#12477=CARTESIAN_POINT('Ctrl Pts',(89.3805570394582,-0.605007279598262,
-4.38853760211599));
#12478=CARTESIAN_POINT('Ctrl Pts',(89.3796568223334,-0.624933910886723,
-4.38571251004663));
#12479=CARTESIAN_POINT('Ctrl Pts',(89.3787573274687,-0.644842433755186,
-4.38275699670061));
#12480=CARTESIAN_POINT('Ctrl Pts',(89.3778578691136,-0.664731277729952,
-4.37967264392692));
#12481=CARTESIAN_POINT('Ctrl Pts',(89.370312436378,-0.831576061088442,-4.35379843168113));
#12482=CARTESIAN_POINT('Ctrl Pts',(89.3627694916172,-0.997038937407362,
-4.3188612788562));
#12483=CARTESIAN_POINT('Ctrl Pts',(89.3552236782343,-1.16012719389742,-4.27507484043943));
#12484=CARTESIAN_POINT('Ctrl Pts',(89.3514222905434,-1.24228688421828,-4.25301635322521));
#12485=CARTESIAN_POINT('Ctrl Pts',(89.3476201903182,-1.32384343025632,-4.2287112733854));
#12486=CARTESIAN_POINT('Ctrl Pts',(89.3438167633393,-1.4046668649752,-4.20218277744718));
#12487=CARTESIAN_POINT('Ctrl Pts',(89.3388999276965,-1.50915041278619,-4.16788837529321));
#12488=CARTESIAN_POINT('Ctrl Pts',(89.3341006624582,-1.61234760269368,-4.12967926390135));
#12489=CARTESIAN_POINT('Ctrl Pts',(89.3295154930798,-1.71384201048532,-4.08747165098001));
#12490=CARTESIAN_POINT('Ctrl Pts',(89.328805309349,-1.72956218813386,-4.08093423490279));
#12491=CARTESIAN_POINT('Ctrl Pts',(89.3281002617829,-1.74524142451454,-4.07430093925114));
#12492=CARTESIAN_POINT('Ctrl Pts',(89.3274007090456,-1.76087807294772,-4.06757150451766));
#12493=CARTESIAN_POINT('Ctrl Pts',(89.3221790911871,-1.87759350889313,-4.01734150082212));
#12494=CARTESIAN_POINT('Ctrl Pts',(89.3170180067439,-1.99210299405547,-3.96214565755558));
#12495=CARTESIAN_POINT('Ctrl Pts',(89.3118532957462,-2.10394889892861,-3.90218784561099));
#12496=CARTESIAN_POINT('Ctrl Pts',(89.3066854717779,-2.21586221764339,-3.8421938947801));
#12497=CARTESIAN_POINT('Ctrl Pts',(89.3015136565798,-2.32510848812348,-3.77743193022012));
#12498=CARTESIAN_POINT('Ctrl Pts',(89.2962574801352,-2.43124102518457,-3.70814962596672));
#12499=CARTESIAN_POINT('Ctrl Pts',(89.2913965944474,-2.52939186464553,-3.6440776975029));
#12500=CARTESIAN_POINT('Ctrl Pts',(89.2864631150228,-2.62488007739734,-3.57613942144677));
#12501=CARTESIAN_POINT('Ctrl Pts',(89.2813859570345,-2.71736351929902,-3.50456902506535));
#12502=CARTESIAN_POINT('Ctrl Pts',(89.280965182924,-2.7250281691072,-3.49863756302613));
#12503=CARTESIAN_POINT('Ctrl Pts',(89.2805434219692,-2.73267221049811,-3.49268115218793));
#12504=CARTESIAN_POINT('Ctrl Pts',(89.2801206337067,-2.74029546476355,-3.48669992454199));
#12505=CARTESIAN_POINT('Ctrl Pts',(89.2776303505565,-2.78519751936587,-3.45146964086056));
#12506=CARTESIAN_POINT('Ctrl Pts',(89.2751043453965,-2.82937745257098,-3.41537913983434));
#12507=CARTESIAN_POINT('Ctrl Pts',(89.272534204999,-2.87279726675529,-3.37845914541868));
#12508=CARTESIAN_POINT('Ctrl Pts',(89.272532154234,-2.87283191226985,-3.37842968623679));
#12509=CARTESIAN_POINT('Ctrl Pts',(89.2725301034409,-2.87286655730067,-3.37840022652676));
#12510=CARTESIAN_POINT('Ctrl Pts',(89.2725280526196,-2.8729012018477,-3.37837076628866));
#12511=CARTESIAN_POINT('Ctrl Pts',(89.267394586954,-2.95962089722541,-3.3046280537393));
#12512=CARTESIAN_POINT('Ctrl Pts',(89.2620740500415,-3.04355784971649,-3.22735275435274));
#12513=CARTESIAN_POINT('Ctrl Pts',(89.2566412400769,-3.12443440269525,-3.14681070859945));
#12514=CARTESIAN_POINT('Ctrl Pts',(89.2561104809455,-3.13233564888054,-3.13894214214445));
#12515=CARTESIAN_POINT('Ctrl Pts',(89.2555786502419,-3.1402076796009,-3.13104243735842));
#12516=CARTESIAN_POINT('Ctrl Pts',(89.2550458177106,-3.14805023258091,-3.12311186850192));
#12517=CARTESIAN_POINT('Ctrl Pts',(89.2490662896212,-3.23606056055093,-3.03411381291612));
#12518=CARTESIAN_POINT('Ctrl Pts',(89.2429611108263,-3.3203597317995,-2.94122308399473));
#12519=CARTESIAN_POINT('Ctrl Pts',(89.2368189778671,-3.40062431570516,-2.84481744754777));
#12520=CARTESIAN_POINT('Ctrl Pts',(89.230524199038,-3.48288365571837,-2.74601591339912));
#12521=CARTESIAN_POINT('Ctrl Pts',(89.2241910551195,-3.56090549561551,-2.64352276011619));
#12522=CARTESIAN_POINT('Ctrl Pts',(89.2178971949538,-3.63438366563388,-2.53776568946566));
#12523=CARTESIAN_POINT('Ctrl Pts',(89.2130203306477,-3.69131900502992,-2.45581870154376));
#12524=CARTESIAN_POINT('Ctrl Pts',(89.2081671301908,-3.74552798451576,-2.37190969139733));
#12525=CARTESIAN_POINT('Ctrl Pts',(89.203450944175,-3.79675155356332,-2.2861754455767));
#12526=CARTESIAN_POINT('Ctrl Pts',(89.2022381243405,-3.80992426565039,-2.26412792805309));
#12527=CARTESIAN_POINT('Ctrl Pts',(89.2010343655256,-3.82289941671646,-2.24195993893644));
#12528=CARTESIAN_POINT('Ctrl Pts',(89.1998415954324,-3.83567234774371,-2.2196743013848));
#12529=CARTESIAN_POINT('Ctrl Pts',(89.1951763176034,-3.88563107178533,-2.13250855891273));
#12530=CARTESIAN_POINT('Ctrl Pts',(89.1906487149425,-3.93253987688793,-2.04357290095941));
#12531=CARTESIAN_POINT('Ctrl Pts',(89.1861496000012,-3.9764769173674,-1.95319328049147));
#12532=CARTESIAN_POINT('Ctrl Pts',(89.1850273570829,-3.98743641344001,-1.93064931565556));
#12533=CARTESIAN_POINT('Ctrl Pts',(89.183906886628,-3.99821112416203,-1.90801528272099));
#12534=CARTESIAN_POINT('Ctrl Pts',(89.1827864940954,-4.00880247330086,-1.88529578119841));
#12535=CARTESIAN_POINT('Ctrl Pts',(89.1748845966895,-4.08350107387963,-1.72505982378282));
#12536=CARTESIAN_POINT('Ctrl Pts',(89.1669864847308,-4.14908402662789,-1.5605718235667));
#12537=CARTESIAN_POINT('Ctrl Pts',(89.1590869820462,-4.20512713898647,-1.39293918911362));
#12538=CARTESIAN_POINT('Ctrl Pts',(89.1555023501855,-4.23055835081728,-1.31687094705638));
#12539=CARTESIAN_POINT('Ctrl Pts',(89.1519174478846,-4.25402437590823,-1.24015520149134));
#12540=CARTESIAN_POINT('Ctrl Pts',(89.148331846413,-4.2754819634251,-1.16289553034143));
#12541=CARTESIAN_POINT('Ctrl Pts',(89.1427150953485,-4.3090947138875,-1.04187027318577));
#12542=CARTESIAN_POINT('Ctrl Pts',(89.1372836934939,-4.33746672531892,-0.919420208707981));
#12543=CARTESIAN_POINT('Ctrl Pts',(89.1321181629932,-4.36026314630882,-0.796029961547062));
#12544=CARTESIAN_POINT('Ctrl Pts',(89.1269499946497,-4.38307120857622,-0.672576703613198));
#12545=CARTESIAN_POINT('Ctrl Pts',(89.1218422568243,-4.40064724792524,-0.548252281346481));
#12546=CARTESIAN_POINT('Ctrl Pts',(89.1167340340962,-4.41291781279323,-0.42354027505825));
#12547=CARTESIAN_POINT('Ctrl Pts',(89.1116198553237,-4.42520268479577,-0.298682858067726));
#12548=CARTESIAN_POINT('Ctrl Pts',(89.1065048462763,-4.43216934172322,-0.173437033166085));
#12549=CARTESIAN_POINT('Ctrl Pts',(89.1013127266966,-4.43378718263489,-0.0483001100602392));
#12550=CARTESIAN_POINT('Ctrl Pts',(89.1006065026572,-4.43400723884241,-0.0312791801777059));
#12551=CARTESIAN_POINT('Ctrl Pts',(89.0998988341112,-4.43412840683536,-0.0142602819635385));
#12552=CARTESIAN_POINT('Ctrl Pts',(89.0991895136419,-4.43415067741398,0.00275531765885942));
#12553=CARTESIAN_POINT('',(87.8465491621224,-4.4326266415555,-0.00371887732998788));
#12554=CARTESIAN_POINT('Ctrl Pts',(89.0991895136049,-4.43415067741516,0.002755318546424));
#12555=CARTESIAN_POINT('Ctrl Pts',(89.0940584661118,-4.43431177720561,0.125841925458626));
#12556=CARTESIAN_POINT('Ctrl Pts',(89.0888408531867,-4.42929579503223,0.248794764078206));
#12557=CARTESIAN_POINT('Ctrl Pts',(89.0834488483057,-4.41909585617478,0.371254491423685));
#12558=CARTESIAN_POINT('Ctrl Pts',(89.0812972309806,-4.41502568827878,0.420120632462279));
#12559=CARTESIAN_POINT('Ctrl Pts',(89.0791178449291,-4.4101299607236,0.468908825028051));
#12560=CARTESIAN_POINT('Ctrl Pts',(89.0769051096917,-4.40440763049221,0.517598479163535));
#12561=CARTESIAN_POINT('Ctrl Pts',(89.0769030860234,-4.40440239710597,0.517643008534498));
#12562=CARTESIAN_POINT('Ctrl Pts',(89.0769010623273,-4.40439716302833,0.517687537823121));
#12563=CARTESIAN_POINT('Ctrl Pts',(89.0768990386032,-4.40439192825929,0.517732067029408));
#12564=CARTESIAN_POINT('Ctrl Pts',(89.0717108190989,-4.39097155572819,0.631891551906531));
#12565=CARTESIAN_POINT('Ctrl Pts',(89.0663335032324,-4.37298416348157,0.745663962758008));
#12566=CARTESIAN_POINT('Ctrl Pts',(89.0608439791029,-4.35050280379623,0.858666722074836));
#12567=CARTESIAN_POINT('Ctrl Pts',(89.0602882381941,-4.34822686676297,0.870106740311668));
#12568=CARTESIAN_POINT('Ctrl Pts',(89.0597313472792,-4.3459049034978,0.88153884000792));
#12569=CARTESIAN_POINT('Ctrl Pts',(89.059173386134,-4.34353701162595,0.892962604077999));
#12570=CARTESIAN_POINT('Ctrl Pts',(89.0531113618511,-4.31781081518433,1.01707722352647));
#12571=CARTESIAN_POINT('Ctrl Pts',(89.0469235432333,-4.28665918413459,1.14021231604018));
#12572=CARTESIAN_POINT('Ctrl Pts',(89.0407014325302,-4.25022497621635,1.2618801082538));
#12573=CARTESIAN_POINT('Ctrl Pts',(89.0344853528745,-4.21382608371527,1.38342996874662));
#12574=CARTESIAN_POINT('Ctrl Pts',(89.0282353979775,-4.17215519818587,1.50351550910955));
#12575=CARTESIAN_POINT('Ctrl Pts',(89.0220254139412,-4.12539113653842,1.62167231983811));
#12576=CARTESIAN_POINT('Ctrl Pts',(89.0173485759035,-4.09017237574424,1.71065809880283));
#12577=CARTESIAN_POINT('Ctrl Pts',(89.0126945260154,-4.05206364381119,1.7985526796479));
#12578=CARTESIAN_POINT('Ctrl Pts',(89.0081811492928,-4.0110095527276,1.88508764521091));
#12579=CARTESIAN_POINT('Ctrl Pts',(89.0067059079872,-3.99759062170222,1.9133724446919));
#12580=CARTESIAN_POINT('Ctrl Pts',(89.0052456958246,-3.98385719741542,1.94151161348086));
#12581=CARTESIAN_POINT('Ctrl Pts',(89.0038046294465,-3.9698079180284,1.96949471348206));
#12582=CARTESIAN_POINT('Ctrl Pts',(88.9988257358338,-3.92126756730704,2.06617650412137));
#12583=CARTESIAN_POINT('Ctrl Pts',(88.9939667019039,-3.86912750892133,2.16107532962121));
#12584=CARTESIAN_POINT('Ctrl Pts',(88.989126359296,-3.81371772843866,2.25403148593715));
#12585=CARTESIAN_POINT('Ctrl Pts',(88.9882817194165,-3.80404872066293,2.27025233702862));
#12586=CARTESIAN_POINT('Ctrl Pts',(88.9874376486925,-3.79428007802033,2.28641414022231));
#12587=CARTESIAN_POINT('Ctrl Pts',(88.9865936095589,-3.78441346018295,2.30251617972391));
#12588=CARTESIAN_POINT('Ctrl Pts',(88.9790454423553,-3.69617717089062,2.44651529259893));
#12589=CARTESIAN_POINT('Ctrl Pts',(88.9714997196197,-3.60010770911251,2.58573895241691));
#12590=CARTESIAN_POINT('Ctrl Pts',(88.9639510940841,-3.49678444365902,2.71935321020572));
#12591=CARTESIAN_POINT('Ctrl Pts',(88.9601386366122,-3.4446006979513,2.78683551848134));
#12592=CARTESIAN_POINT('Ctrl Pts',(88.9563254547329,-3.39056617040065,2.85288623395623));
#12593=CARTESIAN_POINT('Ctrl Pts',(88.9525109323959,-3.33475286920143,2.91739344910565));
#12594=CARTESIAN_POINT('Ctrl Pts',(88.9472306677637,-3.25749313015944,3.00668776608181));
#12595=CARTESIAN_POINT('Ctrl Pts',(88.9421023660308,-3.17661953470607,3.09285158050349));
#12596=CARTESIAN_POINT('Ctrl Pts',(88.9372143103819,-3.09227639170099,3.175404546789));
#12597=CARTESIAN_POINT('Ctrl Pts',(88.9368392356173,-3.08580449637623,3.18173907663354));
#12598=CARTESIAN_POINT('Ctrl Pts',(88.9364655754075,-3.0793121923559,3.18805233001413));
#12599=CARTESIAN_POINT('Ctrl Pts',(88.9360933696384,-3.07279955490985,3.19434408214872));
#12600=CARTESIAN_POINT('Ctrl Pts',(88.9308649365839,-2.98131551105713,3.28272531524506));
#12601=CARTESIAN_POINT('Ctrl Pts',(88.9256960264991,-2.88609324516521,3.3671459059386));
#12602=CARTESIAN_POINT('Ctrl Pts',(88.9205222252319,-2.78749823238605,3.44726151214697));
#12603=CARTESIAN_POINT('Ctrl Pts',(88.915345284881,-2.68884339937208,3.52742572663926));
#12604=CARTESIAN_POINT('Ctrl Pts',(88.9101630841282,-2.58681154263463,3.60327937580524));
#12605=CARTESIAN_POINT('Ctrl Pts',(88.904895067653,-2.48180444078077,3.67450512558962));
#12606=CARTESIAN_POINT('Ctrl Pts',(88.9000293782515,-2.38481690382521,3.74029124783699));
#12607=CARTESIAN_POINT('Ctrl Pts',(88.895090034108,-2.28529074647613,3.80212958643056));
#12608=CARTESIAN_POINT('Ctrl Pts',(88.8900061685127,-2.18357361175643,3.85979509254691));
#12609=CARTESIAN_POINT('Ctrl Pts',(88.8895779133094,-2.17500515309208,3.86465272550009));
#12610=CARTESIAN_POINT('Ctrl Pts',(88.8891486325734,-2.16642113361103,3.86948077528753));
#12611=CARTESIAN_POINT('Ctrl Pts',(88.8887182839436,-2.15782175335337,3.87427912243183));
#12612=CARTESIAN_POINT('Ctrl Pts',(88.8862969240186,-2.10943727320232,3.90127706009769));
#12613=CARTESIAN_POINT('Ctrl Pts',(88.8838416834989,-2.06056752652318,3.92733415410425));
#12614=CARTESIAN_POINT('Ctrl Pts',(88.8813448941584,-2.01125180454248,3.95242916661114));
#12615=CARTESIAN_POINT('Ctrl Pts',(88.8813428564613,-2.01121155665288,3.95244964732707));
#12616=CARTESIAN_POINT('Ctrl Pts',(88.8813408187366,-2.01117130846618,3.95247012740235));
#12617=CARTESIAN_POINT('Ctrl Pts',(88.8813387809842,-2.01113105998239,3.952490606837));
#12618=CARTESIAN_POINT('Ctrl Pts',(88.8761543330759,-1.90873090269395,4.00459436658136));
#12619=CARTESIAN_POINT('Ctrl Pts',(88.8707803904864,-1.80412184797462,4.05268645179417));
#12620=CARTESIAN_POINT('Ctrl Pts',(88.8652938432659,-1.6976623971288,4.09661557354543));
#12621=CARTESIAN_POINT('Ctrl Pts',(88.8647369133398,-1.68685588226361,4.10107474277323));
#12622=CARTESIAN_POINT('Ctrl Pts',(88.8641788231435,-1.67603034427544,4.10549102673119));
#12623=CARTESIAN_POINT('Ctrl Pts',(88.863619653099,-1.66518618723406,4.10986427424895));
#12624=CARTESIAN_POINT('Ctrl Pts',(88.8575592812349,-1.54765552752052,4.15726221065757));
#12625=CARTESIAN_POINT('Ctrl Pts',(88.8513726000233,-1.42793185514377,4.19960391981595));
#12626=CARTESIAN_POINT('Ctrl Pts',(88.8451512083656,-1.3065001605735,4.23673776581859));
#12627=CARTESIAN_POINT('Ctrl Pts',(88.8389358695328,-1.18518660753971,4.27383548410649));
#12628=CARTESIAN_POINT('Ctrl Pts',(88.8326862385821,-1.0621684332796,4.30573583380955));
#12629=CARTESIAN_POINT('Ctrl Pts',(88.8264762691896,-0.937931122903868,
4.33233007236424));
#12630=CARTESIAN_POINT('Ctrl Pts',(88.8217562731814,-0.843502379062377,
4.35254348919164));
#12631=CARTESIAN_POINT('Ctrl Pts',(88.817059309445,-0.74836641143597,4.36969206864705));
#12632=CARTESIAN_POINT('Ctrl Pts',(88.8125022748401,-0.652722061934351,
4.38358287260651));
#12633=CARTESIAN_POINT('Ctrl Pts',(88.8110680851599,-0.622620877519621,
4.38795458566464));
#12634=CARTESIAN_POINT('Ctrl Pts',(88.8096477552705,-0.592469722812713,
4.39200356834735));
#12635=CARTESIAN_POINT('Ctrl Pts',(88.8082449291489,-0.562275860701015,
4.39572370546327));
#12636=CARTESIAN_POINT('Ctrl Pts',(88.8033379360349,-0.456659725396665,
4.40873649937259));
#12637=CARTESIAN_POINT('Ctrl Pts',(88.7985549211245,-0.350544966988067,
4.41788031960409));
#12638=CARTESIAN_POINT('Ctrl Pts',(88.7937928824806,-0.244235520955601,
4.42334373127186));
#12639=CARTESIAN_POINT('Ctrl Pts',(88.7928699688644,-0.223632068817665,
4.42440257547628));
#12640=CARTESIAN_POINT('Ctrl Pts',(88.7919478431361,-0.203021146921662,
4.42532318213354));
#12641=CARTESIAN_POINT('Ctrl Pts',(88.7910257554883,-0.182404741442705,
4.42610692012007));
#12642=CARTESIAN_POINT('Ctrl Pts',(88.7834775121547,-0.0136380893970825,
4.43252262804751));
#12643=CARTESIAN_POINT('Ctrl Pts',(88.7759317389052,0.155498224570251,4.42977097023969));
#12644=CARTESIAN_POINT('Ctrl Pts',(88.7683830849804,0.323988656491828,4.41787215803026));
#12645=CARTESIAN_POINT('Ctrl Pts',(88.7645729185807,0.409033829944684,4.41186625884243));
#12646=CARTESIAN_POINT('Ctrl Pts',(88.7607620340732,0.493914102679781,4.403529109817));
#12647=CARTESIAN_POINT('Ctrl Pts',(88.7569498153798,0.57849664240472,4.39285864372773));
#12648=CARTESIAN_POINT('Ctrl Pts',(88.7516104338553,0.696962681795999,4.37791362244832));
#12649=CARTESIAN_POINT('Ctrl Pts',(88.7464282187022,0.814813527402178,4.35811550109011));
#12650=CARTESIAN_POINT('Ctrl Pts',(88.7414901855034,0.931554253797117,4.33332050942411));
#12651=CARTESIAN_POINT('Ctrl Pts',(88.741171223872,0.939094869877251,4.33171893027827));
#12652=CARTESIAN_POINT('Ctrl Pts',(88.7408532810254,0.946630837061738,4.33009650850236));
#12653=CARTESIAN_POINT('Ctrl Pts',(88.7405363804139,0.954162014877631,4.32845320779207));
#12654=CARTESIAN_POINT('Ctrl Pts',(88.7353078032711,1.07841972458532,4.3013402133026));
#12655=CARTESIAN_POINT('Ctrl Pts',(88.7301389971226,1.20145511200285,4.26892201973708));
#12656=CARTESIAN_POINT('Ctrl Pts',(88.724965633424,1.32277915137856,4.23131177478354));
#12657=CARTESIAN_POINT('Ctrl Pts',(88.7197891379548,1.44417663601871,4.19367876192349));
#12658=CARTESIAN_POINT('Ctrl Pts',(88.7146077169301,1.56386050606829,4.15084706101972));
#12659=CARTESIAN_POINT('Ctrl Pts',(88.7093408739182,1.68134408896872,4.10297497781955));
#12660=CARTESIAN_POINT('Ctrl Pts',(88.7044744759562,1.78989523946017,4.05874267250923));
#12661=CARTESIAN_POINT('Ctrl Pts',(88.6995347059271,1.89656841241729,4.010207035418));
#12662=CARTESIAN_POINT('Ctrl Pts',(88.6944506333384,2.00098330039062,3.95753266766142));
#12663=CARTESIAN_POINT('Ctrl Pts',(88.6940243924115,2.00973728606966,3.95311652864194));
#12664=CARTESIAN_POINT('Ctrl Pts',(88.6935971371976,2.01847542860371,3.94867130287051));
#12665=CARTESIAN_POINT('Ctrl Pts',(88.693168825898,2.02719752046672,3.94419708918269));
#12666=CARTESIAN_POINT('Ctrl Pts',(88.690736229254,2.07673469451726,3.91878576519375));
#12667=CARTESIAN_POINT('Ctrl Pts',(88.6882694915977,2.1257531106961,3.89243994260321));
#12668=CARTESIAN_POINT('Ctrl Pts',(88.6857608276608,2.17421273004713,3.86518085028478));
#12669=CARTESIAN_POINT('Ctrl Pts',(88.6857587910729,2.17425207061955,3.86515872076107));
#12670=CARTESIAN_POINT('Ctrl Pts',(88.6857567544573,2.17429141082386,3.8651365906355));
#12671=CARTESIAN_POINT('Ctrl Pts',(88.6857547178141,2.17433075066006,3.8651144599081));
#12672=CARTESIAN_POINT('Ctrl Pts',(88.6805696920064,2.27448480190595,3.80877253732366));
#12673=CARTESIAN_POINT('Ctrl Pts',(88.6751952198011,2.37252368917428,3.7483670152655));
#12674=CARTESIAN_POINT('Ctrl Pts',(88.6697081700516,2.4681226980108,3.68411251617214));
#12675=CARTESIAN_POINT('Ctrl Pts',(88.6691510908233,2.47782850067427,3.67758900200572));
#12676=CARTESIAN_POINT('Ctrl Pts',(88.6685928511944,2.48750913816589,3.67102585557611));
#12677=CARTESIAN_POINT('Ctrl Pts',(88.6680335316074,2.49716426042529,3.66442332963836));
#12678=CARTESIAN_POINT('Ctrl Pts',(88.6619724941223,2.60179148839528,3.59287540223691));
#12679=CARTESIAN_POINT('Ctrl Pts',(88.6557851745972,2.703425006078,3.51669775867505));
#12680=CARTESIAN_POINT('Ctrl Pts',(88.6495631532013,2.80166966427415,3.43621015540066));
#12681=CARTESIAN_POINT('Ctrl Pts',(88.6433471705941,2.89981897102572,3.35580066944464));
#12682=CARTESIAN_POINT('Ctrl Pts',(88.637096904447,2.9945862542781,3.27108985467447));
#12683=CARTESIAN_POINT('Ctrl Pts',(88.6308862907854,3.08561180252409,3.18242165144434));
#12684=CARTESIAN_POINT('Ctrl Pts',(88.6261587936146,3.15490012816381,3.1149277284998));
#12685=CARTESIAN_POINT('Ctrl Pts',(88.6214543919938,3.22202246743561,3.04513866982926));
#12686=CARTESIAN_POINT('Ctrl Pts',(88.6168898016557,3.28670769553783,2.97311411377379));
#12687=CARTESIAN_POINT('Ctrl Pts',(88.6154621219541,3.30693947546093,2.95058679169539));
#12688=CARTESIAN_POINT('Ctrl Pts',(88.6140481195462,3.32693258699011,2.92784106573228));
#12689=CARTESIAN_POINT('Ctrl Pts',(88.61265136565,3.34667807372635,2.90487957416858));
#12690=CARTESIAN_POINT('Ctrl Pts',(88.6077511753944,3.41595057903976,2.82432445453047));
#12691=CARTESIAN_POINT('Ctrl Pts',(88.6029753969762,3.48228774232787,2.74121671052258));
#12692=CARTESIAN_POINT('Ctrl Pts',(88.5982208451739,3.54567884503379,2.65591299564899));
#12693=CARTESIAN_POINT('Ctrl Pts',(88.5972892946892,3.55809894579443,2.63919959757321));
#12694=CARTESIAN_POINT('Ctrl Pts',(88.5963585590483,3.57040604445793,2.62240176864163));
#12695=CARTESIAN_POINT('Ctrl Pts',(88.5954278621686,3.5826001872094,2.605521994311));
#12696=CARTESIAN_POINT('Ctrl Pts',(88.5878790824142,3.68150553430708,2.46861200620224));
#12697=CARTESIAN_POINT('Ctrl Pts',(88.5803327708345,3.77298476484709,2.32631169387097));
#12698=CARTESIAN_POINT('Ctrl Pts',(88.5727835775853,3.85649165180118,2.17947751716839));
#12699=CARTESIAN_POINT('Ctrl Pts',(88.5689718689625,3.89865561694978,2.10533858881252));
#12700=CARTESIAN_POINT('Ctrl Pts',(88.5651594415353,3.93878622924592,2.03004362944537));
#12701=CARTESIAN_POINT('Ctrl Pts',(88.5613456788694,3.97680804529936,1.95370216437051));
#12702=CARTESIAN_POINT('Ctrl Pts',(88.5556603598935,4.03348859184737,1.83989708050399));
#12703=CARTESIAN_POINT('Ctrl Pts',(88.5501573255947,4.08519648762396,1.72361895994459));
#12704=CARTESIAN_POINT('Ctrl Pts',(88.5449329669845,4.13146929417268,1.60527672236151));
#12705=CARTESIAN_POINT('Ctrl Pts',(88.5397030542424,4.1777912943724,1.48680867251054));
#12706=CARTESIAN_POINT('Ctrl Pts',(88.5345327817112,4.2190184935044,1.36641641112919));
#12707=CARTESIAN_POINT('Ctrl Pts',(88.5293577937609,4.25497390592655,1.24456982842773));
#12708=CARTESIAN_POINT('Ctrl Pts',(88.5241796709027,4.29095109944351,1.1226494334184));
#12709=CARTESIAN_POINT('Ctrl Pts',(88.5189964640541,4.32164971921428,0.999272922515912));
#12710=CARTESIAN_POINT('Ctrl Pts',(88.5137276562027,4.34693167389145,0.874933274360714));
#12711=CARTESIAN_POINT('Ctrl Pts',(88.5088601667149,4.370287934376,0.76006441837417));
#12712=CARTESIAN_POINT('Ctrl Pts',(88.5039191737815,4.38902129238268,0.644373038264876));
#12713=CARTESIAN_POINT('Ctrl Pts',(88.4988337726266,4.40305791118607,0.528266872988238));
#12714=CARTESIAN_POINT('Ctrl Pts',(88.4984066063687,4.40423696663214,0.518514124950444));
#12715=CARTESIAN_POINT('Ctrl Pts',(88.4979784212019,4.40538290308052,0.508758427343947));
#12716=CARTESIAN_POINT('Ctrl Pts',(88.4975491751029,4.40649568756069,0.499000008966845));
#12717=CARTESIAN_POINT('Ctrl Pts',(88.4951269290217,4.41277515719891,0.443933018899884));
#12718=CARTESIAN_POINT('Ctrl Pts',(88.4926708248137,4.41799884925738,0.388780533792759));
#12719=CARTESIAN_POINT('Ctrl Pts',(88.4901731862196,4.42216229197357,0.333587031036786));
#12720=CARTESIAN_POINT('Ctrl Pts',(88.4901711523942,4.42216568226218,0.33354208700451));
#12721=CARTESIAN_POINT('Ctrl Pts',(88.4901691185412,4.42216907184788,0.333497142944872));
#12722=CARTESIAN_POINT('Ctrl Pts',(88.4901670846607,4.4221724607307,0.333452198857978));
#12723=CARTESIAN_POINT('Ctrl Pts',(88.4849814679223,4.43081281462189,0.21886198214381));
#12724=CARTESIAN_POINT('Ctrl Pts',(88.4796064741109,4.43489854926796,0.103778888302272));
#12725=CARTESIAN_POINT('Ctrl Pts',(88.4741189831289,4.43442821784785,-0.0114078262371407));
#12726=CARTESIAN_POINT('Ctrl Pts',(88.4735622701539,4.43438050212403,-0.0230936656757789));
#12727=CARTESIAN_POINT('Ctrl Pts',(88.4730043993173,4.43428591921341,-0.0347805354675403));
#12728=CARTESIAN_POINT('Ctrl Pts',(88.472445450895,4.43414448530773,-0.0464680050712581));
#12729=CARTESIAN_POINT('Ctrl Pts',(88.4663843784788,4.43261081760191,-0.173203490504955));
#12730=CARTESIAN_POINT('Ctrl Pts',(88.4601971327827,4.42556499904317,-0.300014605638085));
#12731=CARTESIAN_POINT('Ctrl Pts',(88.4539752809605,4.41305400745871,-0.426395274606113));
#12732=CARTESIAN_POINT('Ctrl Pts',(88.4477594703326,4.40055516359727,-0.552653232488251));
#12733=CARTESIAN_POINT('Ctrl Pts',(88.4415094715515,4.3826021227949,-0.678481647775574));
#12734=CARTESIAN_POINT('Ctrl Pts',(88.4352992044174,4.35928163403119,-0.803390517563371));
#12735=CARTESIAN_POINT('Ctrl Pts',(88.4305863657173,4.34158421464844,-0.898181183216139));
#12736=CARTESIAN_POINT('Ctrl Pts',(88.4258965276388,4.32079504824394,-0.992445189586246));
#12737=CARTESIAN_POINT('Ctrl Pts',(88.4213467444025,4.29681199588026,-1.08592553637779));
#12738=CARTESIAN_POINT('Ctrl Pts',(88.4199054548131,4.28921459576327,-1.11553843080342));
#12739=CARTESIAN_POINT('Ctrl Pts',(88.4184782198473,4.28129678745296,-1.14507230525));
#12740=CARTESIAN_POINT('Ctrl Pts',(88.4170687605823,4.27305564780333,-1.17451794685169));
#12741=CARTESIAN_POINT('Ctrl Pts',(88.4121482545705,4.24428533978623,-1.27731443067049));
#12742=CARTESIAN_POINT('Ctrl Pts',(88.4073509510985,4.21173177516902,-1.3790745538966));
#12743=CARTESIAN_POINT('Ctrl Pts',(88.4025741940027,4.17568645033873,-1.47958827496848));
#12744=CARTESIAN_POINT('Ctrl Pts',(88.4016654768837,4.1688292869794,-1.49870972854088));
#12745=CARTESIAN_POINT('Ctrl Pts',(88.4007575033423,4.16184569917836,-1.51778621507419));
#12746=CARTESIAN_POINT('Ctrl Pts',(88.3998495666191,4.15473760793157,-1.5368164839011));
#12747=CARTESIAN_POINT('Ctrl Pts',(88.3923010947199,4.0956418299334,-1.69503174912432));
#12748=CARTESIAN_POINT('Ctrl Pts',(88.3847550858854,4.02794349871041,-1.85005612301517));
#12749=CARTESIAN_POINT('Ctrl Pts',(88.3772061906082,3.95205236539545,-2.000960214394));
#12750=CARTESIAN_POINT('Ctrl Pts',(88.3733947719453,3.91373511879901,-2.07715131906201));
#12751=CARTESIAN_POINT('Ctrl Pts',(88.3695826333455,3.87332872318543,-2.152291432711));
#12752=CARTESIAN_POINT('Ctrl Pts',(88.3657691585757,3.83088247457447,-2.22625706203015));
#12753=CARTESIAN_POINT('Ctrl Pts',(88.3603973311197,3.771090831138,-2.33044828456525));
#12754=CARTESIAN_POINT('Ctrl Pts',(88.3551858219174,3.70700415987308,-2.43217120019112));
#12755=CARTESIAN_POINT('Ctrl Pts',(88.3502209500729,3.63868496442522,-2.5309062864685));
#12756=CARTESIAN_POINT('Ctrl Pts',(88.3499314769954,3.63470166568501,-2.53666296059508));
#12757=CARTESIAN_POINT('Ctrl Pts',(88.349642842333,3.63070398855769,-2.54240946675198));
#12758=CARTESIAN_POINT('Ctrl Pts',(88.3493550631941,3.6266919490924,-2.54814569788737));
#12759=CARTESIAN_POINT('Ctrl Pts',(88.344125910758,3.55379032730009,-2.65237711344623));
#12760=CARTESIAN_POINT('Ctrl Pts',(88.3389564100754,3.47646290549643,-2.75343582727919));
#12761=CARTESIAN_POINT('Ctrl Pts',(88.3337821996865,3.39500257058184,-2.85091405116349));
#12762=CARTESIAN_POINT('Ctrl Pts',(88.3286048543391,3.3134928803544,-2.94845133530382));
#12763=CARTESIAN_POINT('Ctrl Pts',(88.3234224307305,3.22784502012949,-3.04240347598096));
#12764=CARTESIAN_POINT('Ctrl Pts',(88.3181544088936,3.13839265625549,-3.13238225347051));
#12765=CARTESIAN_POINT('Ctrl Pts',(88.3132876826322,3.05575439432448,-3.21550682905898));
#12766=CARTESIAN_POINT('Ctrl Pts',(88.3083474564411,2.96986875590525,-3.29524064473898));
#12767=CARTESIAN_POINT('Ctrl Pts',(88.3032628268791,2.88103409455906,-3.37129621597049));
#12768=CARTESIAN_POINT('Ctrl Pts',(88.302835679954,2.87357131836818,-3.37768545298191));
#12769=CARTESIAN_POINT('Ctrl Pts',(88.3024075139372,2.86608772218063,-3.38404876108423));
#12770=CARTESIAN_POINT('Ctrl Pts',(88.3019782867927,2.85858347816145,-3.39038598595353));
#12771=CARTESIAN_POINT('Ctrl Pts',(88.2995531132985,2.81618379788861,-3.42619189892609));
#12772=CARTESIAN_POINT('Ctrl Pts',(88.2970939905493,2.77312586673181,-3.46116442599992));
#12773=CARTESIAN_POINT('Ctrl Pts',(88.2945932112675,2.72944435844312,-3.49527507400002));
#12774=CARTESIAN_POINT('Ctrl Pts',(88.294591175675,2.72940880242658,-3.4953028394965));
#12775=CARTESIAN_POINT('Ctrl Pts',(88.294589140055,2.72937324599686,-3.49533060442208));
#12776=CARTESIAN_POINT('Ctrl Pts',(88.2945871044073,2.72933768915397,-3.49535836877679));
#12777=CARTESIAN_POINT('Ctrl Pts',(88.2894019474456,2.6387680815256,-3.56607912201926));
#12778=CARTESIAN_POINT('Ctrl Pts',(88.2840273641573,2.54526323421544,-3.63328304472224));
#12779=CARTESIAN_POINT('Ctrl Pts',(88.2785402335313,2.44914625265982,-3.69675312843794));
#12780=CARTESIAN_POINT('Ctrl Pts',(88.2779833574119,2.43939156385309,-3.70319455954785));
#12781=CARTESIAN_POINT('Ctrl Pts',(88.2774253220833,2.42961001497231,-3.7095975342355));
#12782=CARTESIAN_POINT('Ctrl Pts',(88.2768662079069,2.41980197365509,-3.71596182704157));
#12783=CARTESIAN_POINT('Ctrl Pts',(88.2708053142631,2.31348112223194,-3.78495185348637));
#12784=CARTESIAN_POINT('Ctrl Pts',(88.264618181701,2.20404118108658,-3.84939661958584));
#12785=CARTESIAN_POINT('Ctrl Pts',(88.2583963889422,2.09192935522711,-3.90905462736617));
#12786=CARTESIAN_POINT('Ctrl Pts',(88.2521806394439,1.97992642418058,-3.96865468900613));
#12787=CARTESIAN_POINT('Ctrl Pts',(88.2459306479155,1.86525694388356,-4.02347763089949));
#12788=CARTESIAN_POINT('Ctrl Pts',(88.239720347209,1.74837679346202,-4.07332396730808));
#12789=CARTESIAN_POINT('Ctrl Pts',(88.2350013663689,1.65956383310872,-4.11120037902767));
#12790=CARTESIAN_POINT('Ctrl Pts',(88.2303054223472,1.56947167411519,-4.14620440265799));
#12791=CARTESIAN_POINT('Ctrl Pts',(88.2257494292195,1.47825849118211,-4.17810865159469));
#12792=CARTESIAN_POINT('Ctrl Pts',(88.2243139504936,1.44951951376367,-4.18816087716407));
#12793=CARTESIAN_POINT('Ctrl Pts',(88.2228923649931,1.42066961783144,-4.19790525660225));
#12794=CARTESIAN_POINT('Ctrl Pts',(88.2214883295742,1.39171478014474,-4.20733437422472));
#12795=CARTESIAN_POINT('Ctrl Pts',(88.2165772771388,1.29043619114185,-4.24031565834308));
#12796=CARTESIAN_POINT('Ctrl Pts',(88.2117899812828,1.18792712012537,-4.26958829497454));
#12797=CARTESIAN_POINT('Ctrl Pts',(88.2070235415891,1.08452252529479,-4.2952790429973));
#12798=CARTESIAN_POINT('Ctrl Pts',(88.2061044428004,1.06458331616579,-4.30023291567912));
#12799=CARTESIAN_POINT('Ctrl Pts',(88.2051861194916,1.04461065704532,-4.30505363710555));
#12800=CARTESIAN_POINT('Ctrl Pts',(88.2042678338922,1.02460673013011,-4.30974215488038));
#12801=CARTESIAN_POINT('Ctrl Pts',(88.1967193233434,0.860170030455247,-4.34828280704974));
#12802=CARTESIAN_POINT('Ctrl Pts',(88.1891732790936,0.693619179579493,-4.37789489650803));
#12803=CARTESIAN_POINT('Ctrl Pts',(88.1816243512325,0.525954872741697,-4.39840418586453));
#12804=CARTESIAN_POINT('Ctrl Pts',(88.1778131454757,0.441306670617002,-4.40875865249864));
#12805=CARTESIAN_POINT('Ctrl Pts',(88.1740012205647,0.356374844747491,-4.41679202056793));
#12806=CARTESIAN_POINT('Ctrl Pts',(88.1701879602425,0.271289481563919,-4.42247685680384));
#12807=CARTESIAN_POINT('Ctrl Pts',(88.1648020783348,0.151114177637051,-4.4305061687426));
#12808=CARTESIAN_POINT('Ctrl Pts',(88.1595777938041,0.0306099578475067,
-4.43356586781557));
#12809=CARTESIAN_POINT('Ctrl Pts',(88.1546011277753,-0.0897524081145261,
-4.431419783972));
#12810=CARTESIAN_POINT('Ctrl Pts',(88.1543247979209,-0.0964355399270603,
-4.43130062246256));
#12811=CARTESIAN_POINT('Ctrl Pts',(88.1540492314834,-0.103118221129596,
-4.43116541296832));
#12812=CARTESIAN_POINT('Ctrl Pts',(88.1537744431882,-0.109800366457727,
-4.43101411574125));
#12813=CARTESIAN_POINT('Ctrl Pts',(88.1485451983774,-0.236962164820039,
-4.42813491654148));
#12814=CARTESIAN_POINT('Ctrl Pts',(88.1433756304472,-0.363937474086309,
-4.41981354439092));
#12815=CARTESIAN_POINT('Ctrl Pts',(88.1382013876067,-0.490224550752052,
-4.40606764837524));
#12816=CARTESIAN_POINT('Ctrl Pts',(88.133024010588,-0.616588122899913,-4.39231342610028));
#12817=CARTESIAN_POINT('Ctrl Pts',(88.1278415902311,-0.742262504656591,
-4.37312772689429));
#12818=CARTESIAN_POINT('Ctrl Pts',(88.1225736131136,-0.866739629134219,
-4.34857298405046));
#12819=CARTESIAN_POINT('Ctrl Pts',(88.1177067342755,-0.981739195275547,
-4.32588781369805));
#12820=CARTESIAN_POINT('Ctrl Pts',(88.1127663851291,-1.0957173703205,-4.29861988600657));
#12821=CARTESIAN_POINT('Ctrl Pts',(88.1076816553335,-1.20826944966748,-4.26685810740331));
#12822=CARTESIAN_POINT('Ctrl Pts',(88.1072547200742,-1.21771979474282,-4.26419125513591));
#12823=CARTESIAN_POINT('Ctrl Pts',(88.1068267669332,-1.22716011473415,-4.26149273092718));
#12824=CARTESIAN_POINT('Ctrl Pts',(88.1063977539355,-1.23659018607998,-4.25876259240397));
#12825=CARTESIAN_POINT('Ctrl Pts',(88.1039716855763,-1.28991723640049,-4.24332365996438));
#12826=CARTESIAN_POINT('Ctrl Pts',(88.1015116496178,-1.34291544842791,-4.22687408587617));
#12827=CARTESIAN_POINT('Ctrl Pts',(88.0990099295383,-1.39554183572812,-4.20942694330022));
#12828=CARTESIAN_POINT('Ctrl Pts',(88.0990078942427,-1.39558465037319,-4.20941274902896));
#12829=CARTESIAN_POINT('Ctrl Pts',(88.0990058589194,-1.39562746477233,-4.2093985540975));
#12830=CARTESIAN_POINT('Ctrl Pts',(88.0990038235686,-1.39567027892551,-4.20938435850586));
#12831=CARTESIAN_POINT('Ctrl Pts',(88.0938185586643,-1.50474372313981,-4.17321963358952));
#12832=CARTESIAN_POINT('Ctrl Pts',(88.088443877551,-1.61251766299464,-4.1326620868654));
#12833=CARTESIAN_POINT('Ctrl Pts',(88.0829566570621,-1.7186323455401,-4.08786031364498));
#12834=CARTESIAN_POINT('Ctrl Pts',(88.0823997816709,-1.72940148730775,-4.08331356633651));
#12835=CARTESIAN_POINT('Ctrl Pts',(88.0818417471935,-1.74015351619585,-4.0787231435896));
#12836=CARTESIAN_POINT('Ctrl Pts',(88.0812826339848,-1.75088804074892,-4.0740892263663));
#12837=CARTESIAN_POINT('Ctrl Pts',(88.0752216516145,-1.86725403435956,-4.02385594595101));
#12838=CARTESIAN_POINT('Ctrl Pts',(88.0690344398818,-1.98156653853143,-3.96850663654002));
#12839=CARTESIAN_POINT('Ctrl Pts',(88.0628125743478,-2.09337661448109,-3.90827959845703));
#12840=CARTESIAN_POINT('Ctrl Pts',(88.056596750375,-2.20507812051486,-3.84811104208423));
#12841=CARTESIAN_POINT('Ctrl Pts',(88.0503466907482,-2.31428226052506,-3.78307453888872));
#12842=CARTESIAN_POINT('Ctrl Pts',(88.0441363251228,-2.4205702515934,-3.71343890046891));
#12843=CARTESIAN_POINT('Ctrl Pts',(88.0394171777067,-2.5013366232805,-3.66052400576866));
#12844=CARTESIAN_POINT('Ctrl Pts',(88.0347210700937,-2.58042157459384,-3.60495175543443));
#12845=CARTESIAN_POINT('Ctrl Pts',(88.0301649114412,-2.65754815888378,-3.54672774048508));
#12846=CARTESIAN_POINT('Ctrl Pts',(88.0287295278983,-2.68184630964094,-3.52838470214167));
#12847=CARTESIAN_POINT('Ctrl Pts',(88.027308034537,-2.70594978116437,-3.50977870841442));
#12848=CARTESIAN_POINT('Ctrl Pts',(88.0259040869341,-2.72984909076715,-3.4909106223017));
#12849=CARTESIAN_POINT('Ctrl Pts',(88.0209928096281,-2.81345344796704,-3.42490644740021));
#12850=CARTESIAN_POINT('Ctrl Pts',(88.0162052789899,-2.89465334862268,-3.3558217680881));
#12851=CARTESIAN_POINT('Ctrl Pts',(88.0114385997259,-2.97336854490301,-3.28400564154297));
#12852=CARTESIAN_POINT('Ctrl Pts',(88.0105196252819,-2.98854415243295,-3.270160114856));
#12853=CARTESIAN_POINT('Ctrl Pts',(88.0096014258522,-3.00362751794813,-3.25621295512458));
#12854=CARTESIAN_POINT('Ctrl Pts',(88.0086832641134,-3.01861822021235,-3.24216650263116));
#12855=CARTESIAN_POINT('Ctrl Pts',(88.0011347006088,-3.1418625934326,-3.12668517273712));
#12856=CARTESIAN_POINT('Ctrl Pts',(87.9935886028726,-3.25884839560788,-3.00449403319924));
#12857=CARTESIAN_POINT('Ctrl Pts',(87.9860396211324,-3.36887579490987,-2.87632928520553));
#12858=CARTESIAN_POINT('Ctrl Pts',(87.9822282302062,-3.42442731771977,-2.81162043116765));
#12859=CARTESIAN_POINT('Ctrl Pts',(87.9784161199724,-3.47820422621604,-2.74538850081591));
#12860=CARTESIAN_POINT('Ctrl Pts',(87.9746026741387,-3.53011155227134,-2.67772655760983));
#12861=CARTESIAN_POINT('Ctrl Pts',(87.9692069018449,-3.60355696725544,-2.58198940690191));
#12862=CARTESIAN_POINT('Ctrl Pts',(87.9639736672022,-3.67303384379134,-2.48321173699712));
#12863=CARTESIAN_POINT('Ctrl Pts',(87.9589887810297,-3.73808305226769,-2.38165655471672));
#12864=CARTESIAN_POINT('Ctrl Pts',(87.9587215274673,-3.74157052060685,-2.37621189995187));
#12865=CARTESIAN_POINT('Ctrl Pts',(87.9584549877401,-3.74504525679008,-2.37075927285087));
#12866=CARTESIAN_POINT('Ctrl Pts',(87.9581891750717,-3.74850718824951,-2.36529871778091));
#12867=CARTESIAN_POINT('Ctrl Pts',(87.9529597979794,-3.8166143449817,-2.25787230441816));
#12868=CARTESIAN_POINT('Ctrl Pts',(87.9477900813474,-3.8800887759405,-2.14758368696896));
#12869=CARTESIAN_POINT('Ctrl Pts',(87.9426156695314,-3.93866697693383,-2.03486023348492));
#12870=CARTESIAN_POINT('Ctrl Pts',(87.9374381231253,-3.99728066382439,-1.92206849362782));
#12871=CARTESIAN_POINT('Ctrl Pts',(87.9322555130345,-4.05099180229852,-1.80683885942346));
#12872=CARTESIAN_POINT('Ctrl Pts',(87.9269873229904,-4.0995706535505,-1.68962879293032));
#12873=CARTESIAN_POINT('Ctrl Pts',(87.9221203438699,-4.14444987255479,-1.58134512404803));
#12874=CARTESIAN_POINT('Ctrl Pts',(87.9171798775052,-4.18494888574857,-1.4713706791475));
#12875=CARTESIAN_POINT('Ctrl Pts',(87.9120950169835,-4.22091730478055,-1.36009155160004));
#12876=CARTESIAN_POINT('Ctrl Pts',(87.9116679621035,-4.22393813274828,-1.35074571128328));
#12877=CARTESIAN_POINT('Ctrl Pts',(87.9112398887284,-4.22692702787906,-1.34139064960208));
#12878=CARTESIAN_POINT('Ctrl Pts',(87.9108107548531,-4.22988391412598,-1.33202658472419));
#12879=CARTESIAN_POINT('Ctrl Pts',(87.9083858750644,-4.2465922052006,-1.27911365248534));
#12880=CARTESIAN_POINT('Ctrl Pts',(87.9059270595241,-4.26227814859569,-1.22591435830625));
#12881=CARTESIAN_POINT('Ctrl Pts',(87.9034266041876,-4.27692881094136,-1.17247165722849));
#12882=CARTESIAN_POINT('Ctrl Pts',(87.9034245691548,-4.27694073460114,-1.17242816209013));
#12883=CARTESIAN_POINT('Ctrl Pts',(87.9034225340943,-4.27695265757532,-1.17238466679047));
#12884=CARTESIAN_POINT('Ctrl Pts',(87.9034204990064,-4.27696457986393,-1.1723411713295));
#12885=CARTESIAN_POINT('Ctrl Pts',(87.8978635917896,-4.30951897158758,-1.05357468933986));
#12886=CARTESIAN_POINT('Ctrl Pts',(87.8920942735389,-4.33701541644651,-0.933385892211736));
#12887=CARTESIAN_POINT('Ctrl Pts',(87.8862035975494,-4.35940446872122,-0.812161221172599));
#12888=CARTESIAN_POINT('Ctrl Pts',(87.8845141711738,-4.36582557480534,-0.777394386774961));
#12889=CARTESIAN_POINT('Ctrl Pts',(87.8828147628401,-4.3718265554393,-0.742542676406213));
#12890=CARTESIAN_POINT('Ctrl Pts',(87.8811075204681,-4.37740620808549,-0.707615996194812));
#12891=CARTESIAN_POINT('Ctrl Pts',(87.8749624100512,-4.39748981317933,-0.581899630484627));
#12892=CARTESIAN_POINT('Ctrl Pts',(87.868716520935,-4.41211541244499,-0.455206027914046));
#12893=CARTESIAN_POINT('Ctrl Pts',(87.8624531612852,-4.42125080253421,-0.327948252047925));
#12894=CARTESIAN_POINT('Ctrl Pts',(87.8610232672522,-4.42333636691305,-0.29889593116357));
#12895=CARTESIAN_POINT('Ctrl Pts',(87.859592462679,-4.42513571081463,-0.269814406401312));
#12896=CARTESIAN_POINT('Ctrl Pts',(87.8581617388014,-4.42664832866523,-0.240708952987256));
#12897=CARTESIAN_POINT('Ctrl Pts',(87.8542856910892,-4.43074623955586,-0.161857870755987));
#12898=CARTESIAN_POINT('Ctrl Pts',(87.8504096358317,-4.43274097879134,-0.0828285532405415));
#12899=CARTESIAN_POINT('Ctrl Pts',(87.846549162128,-4.43262664155567,-0.00371887744496941));
#12900=CARTESIAN_POINT('',(86.595526637467,-4.43203607817194,0.00306014809319887));
#12901=CARTESIAN_POINT('Ctrl Pts',(87.8465491620889,-4.4326266415545,-0.00371887664439084));
#12902=CARTESIAN_POINT('Ctrl Pts',(87.8420321872549,-4.43249286043845,0.0888439646362164));
#12903=CARTESIAN_POINT('Ctrl Pts',(87.837539566186,-4.42947104529508,0.181459192850865));
#12904=CARTESIAN_POINT('Ctrl Pts',(87.8331922601159,-4.42339728692258,0.273914875587774));
#12905=CARTESIAN_POINT('Ctrl Pts',(87.8313277093922,-4.4207922643209,0.313568929702731));
#12906=CARTESIAN_POINT('Ctrl Pts',(87.8294898898659,-4.41762587274885,0.353192984278078));
#12907=CARTESIAN_POINT('Ctrl Pts',(87.8276883450477,-4.41388554911566,0.392767400535123));
#12908=CARTESIAN_POINT('Ctrl Pts',(87.8219800481264,-4.40203412157206,0.518161182690504));
#12909=CARTESIAN_POINT('Ctrl Pts',(87.8163477377429,-4.38491853543299,0.643096989781379));
#12910=CARTESIAN_POINT('Ctrl Pts',(87.8107160151864,-4.36277438570532,0.767152774573604));
#12911=CARTESIAN_POINT('Ctrl Pts',(87.8030492049417,-4.33262819290424,0.936037543346859));
#12912=CARTESIAN_POINT('Ctrl Pts',(87.7953833872014,-4.29316361199279,1.10330118214133));
#12913=CARTESIAN_POINT('Ctrl Pts',(87.787713556523,-4.2446084359225,1.26788955888696));
#12914=CARTESIAN_POINT('Ctrl Pts',(87.7841174992333,-4.22184297965912,1.34505804627621));
#12915=CARTESIAN_POINT('Ctrl Pts',(87.780520582148,-4.19707859508859,1.42163775930275));
#12916=CARTESIAN_POINT('Ctrl Pts',(87.7769223670011,-4.17033599426891,1.49751701101889));
#12917=CARTESIAN_POINT('Ctrl Pts',(87.7721906866967,-4.13516927065124,1.59729880454784));
#12918=CARTESIAN_POINT('Ctrl Pts',(87.7676894420486,-4.09620330819457,1.69572954157321));
#12919=CARTESIAN_POINT('Ctrl Pts',(87.7633106293043,-4.05368569554833,1.79254843599859));
#12920=CARTESIAN_POINT('Ctrl Pts',(87.7624719109063,-4.04554186614788,1.81109314041323));
#12921=CARTESIAN_POINT('Ctrl Pts',(87.761637684244,-4.03726769501056,1.82957885844103));
#12922=CARTESIAN_POINT('Ctrl Pts',(87.7608071903586,-4.02886485861313,1.84800396605026));
#12923=CARTESIAN_POINT('Ctrl Pts',(87.7556353717226,-3.97653702497376,1.96274450366897));
#12924=CARTESIAN_POINT('Ctrl Pts',(87.750515971314,-3.91936486516802,2.07519924701217));
#12925=CARTESIAN_POINT('Ctrl Pts',(87.7453844310164,-3.85756093535738,2.18492081907719));
#12926=CARTESIAN_POINT('Ctrl Pts',(87.7402497364616,-3.79571901588341,2.29470983484027));
#12927=CARTESIAN_POINT('Ctrl Pts',(87.7351025190936,-3.72923934908682,2.40176203210674));
#12928=CARTESIAN_POINT('Ctrl Pts',(87.7298632377616,-3.65837860760412,2.50564268836832));
#12929=CARTESIAN_POINT('Ctrl Pts',(87.7250410517259,-3.59315903713031,2.60125348272576));
#12930=CARTESIAN_POINT('Ctrl Pts',(87.7201404342511,-3.52422787649343,2.69417801339603));
#12931=CARTESIAN_POINT('Ctrl Pts',(87.7150929805591,-3.45182288569065,2.78408983865759));
#12932=CARTESIAN_POINT('Ctrl Pts',(87.7146486095049,-3.44544844739908,2.79200555517738));
#12933=CARTESIAN_POINT('Ctrl Pts',(87.7142031003518,-3.43904708269489,2.799897954217));
#12934=CARTESIAN_POINT('Ctrl Pts',(87.7137564064223,-3.43261895262095,2.80776683238764));
#12935=CARTESIAN_POINT('Ctrl Pts',(87.7118094788342,-3.40460177361932,2.84206355098437));
#12936=CARTESIAN_POINT('Ctrl Pts',(87.709840008583,-3.37607663711951,2.87591290488159));
#12937=CARTESIAN_POINT('Ctrl Pts',(87.7078440961899,-3.34705850668323,2.90929733663113));
#12938=CARTESIAN_POINT('Ctrl Pts',(87.707842060943,-3.3470289166769,2.90933137898782));
#12939=CARTESIAN_POINT('Ctrl Pts',(87.7078400256686,-3.34699932615796,2.9093654208612));
#12940=CARTESIAN_POINT('Ctrl Pts',(87.7078379903667,-3.34696973512643,2.90939946225126));
#12941=CARTESIAN_POINT('Ctrl Pts',(87.7026527277547,-3.27158176980333,2.99612543972864));
#12942=CARTESIAN_POINT('Ctrl Pts',(87.6972780493939,-3.19264053533738,3.07996015897756));
#12943=CARTESIAN_POINT('Ctrl Pts',(87.6917908332701,-3.11042172940336,3.16062886407172));
#12944=CARTESIAN_POINT('Ctrl Pts',(87.6912339754052,-3.10207793763384,3.16881534732183));
#12945=CARTESIAN_POINT('Ctrl Pts',(87.6906759585418,-3.09370043462526,3.17696921727969));
#12946=CARTESIAN_POINT('Ctrl Pts',(87.6901168630286,-3.08528953812638,3.18509018242693));
#12947=CARTESIAN_POINT('Ctrl Pts',(87.6840559043722,-2.99410995477915,3.27312672152846));
#12948=CARTESIAN_POINT('Ctrl Pts',(87.6778687188843,-2.89900014999921,3.35729765775097));
#12949=CARTESIAN_POINT('Ctrl Pts',(87.6716468824007,-2.80035295348696,3.43728048673872));
#12950=CARTESIAN_POINT('Ctrl Pts',(87.6654310880813,-2.70180155546905,3.51718564261601));
#12951=CARTESIAN_POINT('Ctrl Pts',(87.6591810609017,-2.59971984348263,3.59291113138957));
#12952=CARTESIAN_POINT('Ctrl Pts',(87.6529707306469,-2.49451718893161,3.66417402955279));
#12953=CARTESIAN_POINT('Ctrl Pts',(87.6482523398717,-2.41458790749374,3.71831707630076));
#12954=CARTESIAN_POINT('Ctrl Pts',(87.643556983457,-2.33285456524835,3.76988570281975));
#12955=CARTESIAN_POINT('Ctrl Pts',(87.6390015883502,-2.24942888367878,3.81862649461662));
#12956=CARTESIAN_POINT('Ctrl Pts',(87.6375655193732,-2.22312929157413,3.83399182240296));
#12957=CARTESIAN_POINT('Ctrl Pts',(87.6361433597352,-2.19666185259931,3.84907592724259));
#12958=CARTESIAN_POINT('Ctrl Pts',(87.6347387726507,-2.17003102095355,3.86387037446465));
#12959=CARTESIAN_POINT('Ctrl Pts',(87.6298265739827,-2.07689622198936,3.91561032333828));
#12960=CARTESIAN_POINT('Ctrl Pts',(87.6250380662065,-1.98184406908071,3.96394347591442));
#12961=CARTESIAN_POINT('Ctrl Pts',(87.6202703782167,-1.88522772634785,4.00893014210631));
#12962=CARTESIAN_POINT('Ctrl Pts',(87.6193524758796,-1.8666265999769,4.01759123027395));
#12963=CARTESIAN_POINT('Ctrl Pts',(87.6184353452515,-1.84796735203671,4.02612833703379));
#12964=CARTESIAN_POINT('Ctrl Pts',(87.6175182522254,-1.82925229586479,4.03454197231946));
#12965=CARTESIAN_POINT('Ctrl Pts',(87.6099697187913,-1.67520987790019,4.10379406065791));
#12966=CARTESIAN_POINT('Ctrl Pts',(87.6024236510301,-1.51738614938628,4.16468603921365));
#12967=CARTESIAN_POINT('Ctrl Pts',(87.5948746991461,-1.35673006542032,4.21685565374921));
#12968=CARTESIAN_POINT('Ctrl Pts',(87.591063375288,-1.27561782955352,4.24319511114682));
#12969=CARTESIAN_POINT('Ctrl Pts',(87.5872513321114,-1.19378362697453,4.26731029657811));
#12970=CARTESIAN_POINT('Ctrl Pts',(87.5834379533438,-1.11134991493068,4.28914941908763));
#12971=CARTESIAN_POINT('Ctrl Pts',(87.5780485769099,-0.994847901328057,
4.32001423985805));
#12972=CARTESIAN_POINT('Ctrl Pts',(87.5728211362164,-0.877071722791255,
4.3460573951986));
#12973=CARTESIAN_POINT('Ctrl Pts',(87.5678415778635,-0.758439264454936,
4.36695688964637));
#12974=CARTESIAN_POINT('Ctrl Pts',(87.5675684286752,-0.751931787807793,
4.36810331258967));
#12975=CARTESIAN_POINT('Ctrl Pts',(87.567296025358,-0.745421747656629,4.36923425749517));
#12976=CARTESIAN_POINT('Ctrl Pts',(87.5670243820978,-0.738909217522545,
4.37034967100128));
#12977=CARTESIAN_POINT('Ctrl Pts',(87.5617950797062,-0.613538945582386,
4.39182207753265));
#12978=CARTESIAN_POINT('Ctrl Pts',(87.5566254430359,-0.487311806443546,
4.40791682779094));
#12979=CARTESIAN_POINT('Ctrl Pts',(87.5514511172639,-0.36072368253644,4.4185553687992));
#12980=CARTESIAN_POINT('Ctrl Pts',(87.5462736570173,-0.23405887477288,4.42920035436423));
#12981=CARTESIAN_POINT('Ctrl Pts',(87.5410911391898,-0.107032693729212,
4.43438212200354));
#12982=CARTESIAN_POINT('Ctrl Pts',(87.5358230481848,0.0198442128251148,
4.43406487031915));
#12983=CARTESIAN_POINT('Ctrl Pts',(87.5309561347443,0.137059143472471,4.43377177809935));
#12984=CARTESIAN_POINT('Ctrl Pts',(87.5260157390795,0.254147184748634,4.42878522511559));
#12985=CARTESIAN_POINT('Ctrl Pts',(87.5209309533604,0.370694107711927,4.41911514676029));
#12986=CARTESIAN_POINT('Ctrl Pts',(87.5205039336699,0.380481704225322,4.418303054748));
#12987=CARTESIAN_POINT('Ctrl Pts',(87.5200758956512,0.390265510942247,4.41745794660317));
#12988=CARTESIAN_POINT('Ctrl Pts',(87.5196467973071,0.400045297283987,4.41657983617998));
#12989=CARTESIAN_POINT('Ctrl Pts',(87.5172214354079,0.455322884585387,4.41161655540042));
#12990=CARTESIAN_POINT('Ctrl Pts',(87.5147621242226,0.510470886944629,4.4055990652705));
#12991=CARTESIAN_POINT('Ctrl Pts',(87.512261154631,0.56544465342528,4.39853197945318));
#12992=CARTESIAN_POINT('Ctrl Pts',(87.5122591194373,0.565489388979495,4.39852622852831));
#12993=CARTESIAN_POINT('Ctrl Pts',(87.5122570842161,0.565534124418486,4.39852047690849));
#12994=CARTESIAN_POINT('Ctrl Pts',(87.5122550489673,0.565578859742214,4.39851472459374));
#12995=CARTESIAN_POINT('Ctrl Pts',(87.5070697694304,0.679552716391212,4.38385933726274));
#12996=CARTESIAN_POINT('Ctrl Pts',(87.5016950758124,0.793090461968622,4.36464378107407));
#12997=CARTESIAN_POINT('Ctrl Pts',(87.4962078458948,0.905810578361075,4.34094516434875));
#12998=CARTESIAN_POINT('Ctrl Pts',(87.4956509902613,0.917249652860444,4.3385401788774));
#12999=CARTESIAN_POINT('Ctrl Pts',(87.4950929756595,0.928680276631663,4.33608905636515));
#13000=CARTESIAN_POINT('Ctrl Pts',(87.4945338824363,0.940102030899779,4.33359189962059));
#13001=CARTESIAN_POINT('Ctrl Pts',(87.4884729125023,1.06392200643301,4.3065209366357));
#13002=CARTESIAN_POINT('Ctrl Pts',(87.4822857175649,1.18670399204952,4.27403588380812));
#13003=CARTESIAN_POINT('Ctrl Pts',(87.4760638729893,1.30796179006401,4.23628485623563));
#13004=CARTESIAN_POINT('Ctrl Pts',(87.4698480703799,1.42910183593701,4.19857048827936));
#13005=CARTESIAN_POINT('Ctrl Pts',(87.4635980362634,1.54872079402424,4.15560071509786));
#13006=CARTESIAN_POINT('Ctrl Pts',(87.4573876999309,1.66635623553417,4.10755936331984));
#13007=CARTESIAN_POINT('Ctrl Pts',(87.4526693738758,1.7557301983872,4.07105976817992));
#13008=CARTESIAN_POINT('Ctrl Pts',(87.4479740820003,1.84396193431663,4.03163150524466));
#13009=CARTESIAN_POINT('Ctrl Pts',(87.443418752614,1.93077860884527,3.98922704140366));
#13010=CARTESIAN_POINT('Ctrl Pts',(87.4419826161307,1.95814887849518,3.97585839285786));
#13011=CARTESIAN_POINT('Ctrl Pts',(87.4405603908129,1.98537815433257,3.96219410741805));
#13012=CARTESIAN_POINT('Ctrl Pts',(87.439155740593,2.01245694566142,3.94823321505794));
#13013=CARTESIAN_POINT('Ctrl Pts',(87.4342433948206,2.10715695298619,3.89940915224413));
#13014=CARTESIAN_POINT('Ctrl Pts',(87.4294547316289,2.20008468693029,3.84710035194527));
#13015=CARTESIAN_POINT('Ctrl Pts',(87.4246868836489,2.29109450842686,3.79163417302202));
#13016=CARTESIAN_POINT('Ctrl Pts',(87.4237691305853,2.30861279819681,3.78095760450633));
#13017=CARTESIAN_POINT('Ctrl Pts',(87.4228521487585,2.3260601554,3.77016396423666));
#13018=CARTESIAN_POINT('Ctrl Pts',(87.4219352045201,2.3434357221474,3.7592554589208));
#13019=CARTESIAN_POINT('Ctrl Pts',(87.4143866662749,2.48647618701755,3.66945363005947));
#13020=CARTESIAN_POINT('Ctrl Pts',(87.4068405936064,2.62465566138366,3.57186972469084));
#13021=CARTESIAN_POINT('Ctrl Pts',(87.3992916367383,2.75714652993736,3.46709263703067));
#13022=CARTESIAN_POINT('Ctrl Pts',(87.3954802914649,2.82403900984525,3.41419239335634));
#13023=CARTESIAN_POINT('Ctrl Pts',(87.3916682268472,2.88948066590474,3.35945806798491));
#13024=CARTESIAN_POINT('Ctrl Pts',(87.3878548266096,2.95336049953169,3.30296285886929));
#13025=CARTESIAN_POINT('Ctrl Pts',(87.3824646453376,3.04365363988452,3.22310776914367));
#13026=CARTESIAN_POINT('Ctrl Pts',(87.3772364770673,3.13063949483509,3.13951781825546));
#13027=CARTESIAN_POINT('Ctrl Pts',(87.3722562512605,3.21381824072451,3.0523624015897));
#13028=CARTESIAN_POINT('Ctrl Pts',(87.371983837485,3.21836804169512,3.04759508038163));
#13029=CARTESIAN_POINT('Ctrl Pts',(87.3717121655507,3.22290644391039,3.04281710161229));
#13030=CARTESIAN_POINT('Ctrl Pts',(87.3714412495208,3.2274333628932,3.03802849663882));
#13031=CARTESIAN_POINT('Ctrl Pts',(87.366211935062,3.31481351127428,2.94559719519307));
#13032=CARTESIAN_POINT('Ctrl Pts',(87.3610422843428,3.39819330392435,2.84947119216636));
#13033=CARTESIAN_POINT('Ctrl Pts',(87.3558679420249,3.47723242920269,2.75001962188339));
#13034=CARTESIAN_POINT('Ctrl Pts',(87.3506904651807,3.55631943500333,2.65050780557529));
#13035=CARTESIAN_POINT('Ctrl Pts',(87.3455079282499,3.63106015594755,2.54766621272678));
#13036=CARTESIAN_POINT('Ctrl Pts',(87.3402398152633,3.70114167286168,2.44189996909579));
#13037=CARTESIAN_POINT('Ctrl Pts',(87.335372893766,3.76588615387318,2.34418832051926));
#13038=CARTESIAN_POINT('Ctrl Pts',(87.3304324879514,3.82665427084412,2.24398003880654));
#13039=CARTESIAN_POINT('Ctrl Pts',(87.3253476904251,3.88322462821622,2.14162536304834));
#13040=CARTESIAN_POINT('Ctrl Pts',(87.3249206559189,3.88797555379467,2.13302935146696));
#13041=CARTESIAN_POINT('Ctrl Pts',(87.3244926030068,3.89269689942722,2.12441818745693));
#13042=CARTESIAN_POINT('Ctrl Pts',(87.3240634896879,3.89738854879096,2.11579207061174));
#13043=CARTESIAN_POINT('Ctrl Pts',(87.3216382590273,3.92390446285128,2.06703962659732));
#13044=CARTESIAN_POINT('Ctrl Pts',(87.3191790825226,3.94947129899816,2.01781058647708));
#13045=CARTESIAN_POINT('Ctrl Pts',(87.3166782524288,3.97406814418842,1.96814466095132));
#13046=CARTESIAN_POINT('Ctrl Pts',(87.3166762172577,3.97408816105828,1.96810424290746));
#13047=CARTESIAN_POINT('Ctrl Pts',(87.3166741820589,3.97410817728591,1.96806382457419));
#13048=CARTESIAN_POINT('Ctrl Pts',(87.3166721468325,3.97412819287132,1.96802340595155));
#13049=CARTESIAN_POINT('Ctrl Pts',(87.3114868635282,4.02512324822928,1.8650461581332));
#13050=CARTESIAN_POINT('Ctrl Pts',(87.3061121666443,4.0720814299214,1.759903512446));
#13051=CARTESIAN_POINT('Ctrl Pts',(87.3006249341305,4.11485538004488,1.65295572897146));
#13052=CARTESIAN_POINT('Ctrl Pts',(87.3000680823831,4.11919613812506,1.64210252383297));
#13053=CARTESIAN_POINT('Ctrl Pts',(87.2995100716915,4.12349381512763,1.63123077164528));
#13054=CARTESIAN_POINT('Ctrl Pts',(87.2989509824011,4.12774826442953,1.62034087791471));
#13055=CARTESIAN_POINT('Ctrl Pts',(87.2928900141741,4.17386984551746,1.50228585337636));
#13056=CARTESIAN_POINT('Ctrl Pts',(87.2867028218786,4.21491020159689,1.38209288317381));
#13057=CARTESIAN_POINT('Ctrl Pts',(87.280480980815,4.25072302986795,1.26024871219734));
#13058=CARTESIAN_POINT('Ctrl Pts',(87.274265181783,4.28650108029126,1.13852286413002));
#13059=CARTESIAN_POINT('Ctrl Pts',(87.2680151521108,4.31706211786227,1.01514909574692));
#13060=CARTESIAN_POINT('Ctrl Pts',(87.2618048209915,4.34230273810106,0.890614170921266));
#13061=CARTESIAN_POINT('Ctrl Pts',(87.2570866546338,4.36147875995381,0.796001423005591));
#13062=CARTESIAN_POINT('Ctrl Pts',(87.252391521378,4.37758438814031,0.700715537038209));
#13063=CARTESIAN_POINT('Ctrl Pts',(87.2478363532498,4.39042878644756,0.604957194971616));
#13064=CARTESIAN_POINT('Ctrl Pts',(87.2464000699041,4.39447873473821,0.574763773334275));
#13065=CARTESIAN_POINT('Ctrl Pts',(87.2449777018167,4.39820440517015,0.544523766430797));
#13066=CARTESIAN_POINT('Ctrl Pts',(87.2435729145498,4.40159972569208,0.514244537173169));
#13067=CARTESIAN_POINT('Ctrl Pts',(87.2386603570905,4.41347320116494,0.408357719240865));
#13068=CARTESIAN_POINT('Ctrl Pts',(87.2338714695506,4.42146363807649,0.302013713112158));
#13069=CARTESIAN_POINT('Ctrl Pts',(87.2291033900858,4.42576271697741,0.195515259139371));
#13070=CARTESIAN_POINT('Ctrl Pts',(87.2281858778846,4.4265899803178,0.175021970039555));
#13071=CARTESIAN_POINT('Ctrl Pts',(87.2272691361764,4.42728055817177,0.154522806978717));
#13072=CARTESIAN_POINT('Ctrl Pts',(87.2263524320363,4.42783581003968,0.134019705854794));
#13073=CARTESIAN_POINT('Ctrl Pts',(87.2188038983124,4.43240799125576,-0.0348115926004418));
#13074=CARTESIAN_POINT('Ctrl Pts',(87.2112578301234,4.42780862949383,-0.203912158104957));
#13075=CARTESIAN_POINT('Ctrl Pts',(87.2037088776929,4.41406895227369,-0.372266724295081));
#13076=CARTESIAN_POINT('Ctrl Pts',(87.1998975398427,4.40713202263717,-0.457266084974127));
#13077=CARTESIAN_POINT('Ctrl Pts',(87.1960854826396,4.39786434134989,-0.542074925775098));
#13078=CARTESIAN_POINT('Ctrl Pts',(87.1922720898112,4.38626528328757,-0.626560287858358));
#13079=CARTESIAN_POINT('Ctrl Pts',(87.1868829198374,4.36987324128047,-0.745956845476469));
#13080=CARTESIAN_POINT('Ctrl Pts',(87.18165566809,4.34854118073539,-0.864672026658181));
#13081=CARTESIAN_POINT('Ctrl Pts',(87.1766762855012,4.32213291004414,-0.982196215678846));
#13082=CARTESIAN_POINT('Ctrl Pts',(87.1764029378242,4.32068320431873,-0.988647811532593));
#13083=CARTESIAN_POINT('Ctrl Pts',(87.1761303371157,4.31921820531694,-0.995095805879495));
#13084=CARTESIAN_POINT('Ctrl Pts',(87.1758584975946,4.31773789206522,-1.00154011012351));
#13085=CARTESIAN_POINT('Ctrl Pts',(87.1706291943329,4.28926150685784,-1.12550744597788));
#13086=CARTESIAN_POINT('Ctrl Pts',(87.165459555318,4.25549235614025,-1.2481940859127));
#13087=CARTESIAN_POINT('Ctrl Pts',(87.1602852252395,4.21654895949107,-1.36911215257806));
#13088=CARTESIAN_POINT('Ctrl Pts',(87.155107760644,4.17758197162485,-1.49010346925755));
#13089=CARTESIAN_POINT('Ctrl Pts',(87.1499252364988,4.13343412021964,-1.60932387146666));
#13090=CARTESIAN_POINT('Ctrl Pts',(87.1446571368701,4.08426906522461,-1.72628832345511));
#13091=CARTESIAN_POINT('Ctrl Pts',(87.1397902258514,4.03884814216901,-1.83434542569051));
#13092=CARTESIAN_POINT('Ctrl Pts',(87.1348498309491,3.98914481113516,-1.94047754080729));
#13093=CARTESIAN_POINT('Ctrl Pts',(87.1297650447026,3.93532779867126,-2.04430623194306));
#13094=CARTESIAN_POINT('Ctrl Pts',(87.129338013202,3.93080812793682,-2.0530259931345));
#13095=CARTESIAN_POINT('Ctrl Pts',(87.128909963308,3.92625944699761,-2.06172953849333));
#13096=CARTESIAN_POINT('Ctrl Pts',(87.1284808530202,3.92168185746445,-2.07041666055344));
#13097=CARTESIAN_POINT('Ctrl Pts',(87.1260555633436,3.89580976594511,-2.11951543084519));
#13098=CARTESIAN_POINT('Ctrl Pts',(87.1235963261056,3.86901478499991,-2.168088573022));
#13099=CARTESIAN_POINT('Ctrl Pts',(87.1210954329384,3.84131836950711,-2.21609666245408));
#13100=CARTESIAN_POINT('Ctrl Pts',(87.1210933977422,3.84129583050394,-2.21613573084833));
#13101=CARTESIAN_POINT('Ctrl Pts',(87.1210913625185,3.84127329090383,-2.21617479886855));
#13102=CARTESIAN_POINT('Ctrl Pts',(87.1210893272671,3.84125075070682,-2.21621386651472));
#13103=CARTESIAN_POINT('Ctrl Pts',(87.1159040500741,3.78382434531974,-2.3157478006998));
#13104=CARTESIAN_POINT('Ctrl Pts',(87.1105293586286,3.72235764435729,-2.41312273717083));
#13105=CARTESIAN_POINT('Ctrl Pts',(87.1050421308377,3.65706876348978,-2.50801629903429));
#13106=CARTESIAN_POINT('Ctrl Pts',(87.1044852764418,3.65044312269184,-2.51764627961582));
#13107=CARTESIAN_POINT('Ctrl Pts',(87.1039272630813,3.64377816032576,-2.52725069005747));
#13108=CARTESIAN_POINT('Ctrl Pts',(87.103368171103,3.63707413257389,-2.53682918350185));
#13109=CARTESIAN_POINT('Ctrl Pts',(87.0973072046553,3.5643975626333,-2.6406670664137));
#13110=CARTESIAN_POINT('Ctrl Pts',(87.091120013192,3.4871245093646,-2.7414615945206));
#13111=CARTESIAN_POINT('Ctrl Pts',(87.0848981721618,3.405578937502,-2.83882114032578));
#13112=CARTESIAN_POINT('Ctrl Pts',(87.0786823731751,3.32411255472528,-2.93608614005987));
#13113=CARTESIAN_POINT('Ctrl Pts',(87.0724323427522,3.23838221335855,-3.02992308948798));
#13114=CARTESIAN_POINT('Ctrl Pts',(87.0662220102581,3.14873567846447,-3.11997605164627));
#13115=CARTESIAN_POINT('Ctrl Pts',(87.0615037416729,3.08062717867503,-3.18839333248644));
#13116=CARTESIAN_POINT('Ctrl Pts',(87.0568085068176,3.01025603180792,-3.25462847905602));
#13117=CARTESIAN_POINT('Ctrl Pts',(87.0522532353739,2.93768345794995,-3.31841140273829));
#13118=CARTESIAN_POINT('Ctrl Pts',(87.0508170479532,2.91480275392368,-3.33852090307874));
#13119=CARTESIAN_POINT('Ctrl Pts',(87.0493947731304,2.89170351892678,-3.35838639428964));
#13120=CARTESIAN_POINT('Ctrl Pts',(87.0479900754107,2.86838851367361,-3.37799874311116));
#13121=CARTESIAN_POINT('Ctrl Pts',(87.0430776682255,2.78685296497673,-3.44658562975487));
#13122=CARTESIAN_POINT('Ctrl Pts',(87.0382889398302,2.70278417717264,-3.51219462757426));
#13123=CARTESIAN_POINT('Ctrl Pts',(87.0335210244836,2.61654035549795,-3.57481742436555));
#13124=CARTESIAN_POINT('Ctrl Pts',(87.0326033456464,2.59994104023301,-3.58687041003486));
#13125=CARTESIAN_POINT('Ctrl Pts',(87.0316864378192,2.58326102286555,-3.5988128593167));
#13126=CARTESIAN_POINT('Ctrl Pts',(87.0307695675744,2.56650266965896,-3.6106448304546));
#13127=CARTESIAN_POINT('Ctrl Pts',(87.0232210325432,2.42853220222858,-3.7080567043061));
#13128=CARTESIAN_POINT('Ctrl Pts',(87.0156749630928,2.28525257417996,-3.79798508960943));
#13129=CARTESIAN_POINT('Ctrl Pts',(87.0081260094421,2.13752602929942,-3.87989307101794));
#13130=CARTESIAN_POINT('Ctrl Pts',(87.0043146727118,2.06294144014906,-3.92124700064805));
#13131=CARTESIAN_POINT('Ctrl Pts',(87.0005026166394,1.98722314558315,-3.96055559229602));
#13132=CARTESIAN_POINT('Ctrl Pts',(86.9966892249516,1.91048145048875,-3.99774460821275));
#13133=CARTESIAN_POINT('Ctrl Pts',(86.9912997004426,1.80202124486586,-4.05030441039433));
#13134=CARTESIAN_POINT('Ctrl Pts',(86.9860721269399,1.69138886072014,-4.09837461991389));
#13135=CARTESIAN_POINT('Ctrl Pts',(86.981092447861,1.57893298931347,-4.14155930441737));
#13136=CARTESIAN_POINT('Ctrl Pts',(86.980819429462,1.57276742693773,-4.14392696973046));
#13137=CARTESIAN_POINT('Ctrl Pts',(86.9805471562201,1.56659639585105,-4.14627994604861));
#13138=CARTESIAN_POINT('Ctrl Pts',(86.9802756422993,1.56041995793549,-4.14861816704189));
#13139=CARTESIAN_POINT('Ctrl Pts',(86.9750463358532,1.44146293902382,-4.19365185842192));
#13140=CARTESIAN_POINT('Ctrl Pts',(86.9698766938549,1.32063722601068,-4.23357071521643));
#13141=CARTESIAN_POINT('Ctrl Pts',(86.9647023611029,1.19841455402902,-4.26820287365268));
#13142=CARTESIAN_POINT('Ctrl Pts',(86.9595248938412,1.07611784194031,-4.30285601157396));
#13143=CARTESIAN_POINT('Ctrl Pts',(86.9543423673408,0.952422450226131,-4.33221564577044));
#13144=CARTESIAN_POINT('Ctrl Pts',(86.949074265738,0.827822776770507,-4.3561490548337));
#13145=CARTESIAN_POINT('Ctrl Pts',(86.944207350963,0.712711862548233,-4.37825983988892));
#13146=CARTESIAN_POINT('Ctrl Pts',(86.9392669525721,0.596828630513182,-4.39573940968646));
#13147=CARTESIAN_POINT('Ctrl Pts',(86.9341821630361,0.480581574012372,-4.4085183619281));
#13148=CARTESIAN_POINT('Ctrl Pts',(86.9337551334635,0.470818941653778,-4.40959156082378));
#13149=CARTESIAN_POINT('Ctrl Pts',(86.9333270855093,0.461053720111495,-4.4106316263472));
#13150=CARTESIAN_POINT('Ctrl Pts',(86.9328979771739,0.451286138377544,-4.41163852803421));
#13151=CARTESIAN_POINT('Ctrl Pts',(86.9304726880258,0.396080475787726,-4.41732946324301));
#13152=CARTESIAN_POINT('Ctrl Pts',(86.9280134514225,0.340800566886789,-4.42196091961307));
#13153=CARTESIAN_POINT('Ctrl Pts',(86.9255125590039,0.285491117169027,-4.42552889382131));
#13154=CARTESIAN_POINT('Ctrl Pts',(86.9255105238159,0.28544610718554,-4.42553179738411));
#13155=CARTESIAN_POINT('Ctrl Pts',(86.9255084886003,0.285401097182359,-4.42553470024274));
#13156=CARTESIAN_POINT('Ctrl Pts',(86.9255064533572,0.285356087159519,-4.42553760239722));
#13157=CARTESIAN_POINT('Ctrl Pts',(86.9203211737466,0.170682047092974,-4.43293155065508));
#13158=CARTESIAN_POINT('Ctrl Pts',(86.9149464801288,0.0555646764875576,
-4.43576603111863));
#13159=CARTESIAN_POINT('Ctrl Pts',(86.9094592503935,-0.0596068026293469,
-4.43404382642809));
#13160=CARTESIAN_POINT('Ctrl Pts',(86.9089023965005,-0.0712946104312107,
-4.43386905401418));
#13161=CARTESIAN_POINT('Ctrl Pts',(86.9083443836482,-0.0829829395834126,
-4.43364738023689));
#13162=CARTESIAN_POINT('Ctrl Pts',(86.907785292183,-0.0946713593865203,
-4.43337882598583));
#13163=CARTESIAN_POINT('Ctrl Pts',(86.9017243243539,-0.221382534226761,
-4.43046749791641));
#13164=CARTESIAN_POINT('Ctrl Pts',(86.895537131799,-0.348109428700612,-4.4220435073402));
#13165=CARTESIAN_POINT('Ctrl Pts',(86.8893152899021,-0.474346501949595,
-4.40815933176324));
#13166=CARTESIAN_POINT('Ctrl Pts',(86.8830994900267,-0.600460986564145,
-4.39428863908858));
#13167=CARTESIAN_POINT('Ctrl Pts',(86.8768494589391,-0.726086672918377,
-4.37496872859089));
#13168=CARTESIAN_POINT('Ctrl Pts',(86.8706391259347,-0.850734526830391,
-4.35029167322151));
#13169=CARTESIAN_POINT('Ctrl Pts',(86.8659208745263,-0.945434748517955,
-4.33154347547294));
#13170=CARTESIAN_POINT('Ctrl Pts',(86.8612256567654,-1.03957345093702,-4.3097024085963));
#13171=CARTESIAN_POINT('Ctrl Pts',(86.8566704027144,-1.13289191899611,-4.28466967187061));
#13172=CARTESIAN_POINT('Ctrl Pts',(86.8552341984528,-1.16231385243956,-4.27677722004228));
#13173=CARTESIAN_POINT('Ctrl Pts',(86.8538119072514,-1.19165387591231,-4.26856760529915));
#13174=CARTESIAN_POINT('Ctrl Pts',(86.852407193798,-1.22090285747926,-4.26003806115109));
#13175=CARTESIAN_POINT('Ctrl Pts',(86.8474947558015,-1.32318977447885,-4.23020930378668));
#13176=CARTESIAN_POINT('Ctrl Pts',(86.842705994816,-1.42440293531723,-4.19662121719783));
#13177=CARTESIAN_POINT('Ctrl Pts',(86.8379380458908,-1.52433681414696,-4.15956730069596));
#13178=CARTESIAN_POINT('Ctrl Pts',(86.8370203997396,-1.5435702289191,-4.1524358518484));
#13179=CARTESIAN_POINT('Ctrl Pts',(86.836103524496,-1.56275640043473,-4.1451759642625));
#13180=CARTESIAN_POINT('Ctrl Pts',(86.8351866868319,-1.5818940653392,-4.13778963924228));
#13181=CARTESIAN_POINT('Ctrl Pts',(86.8276381514256,-1.73945886310671,-4.07697632613084));
#13182=CARTESIAN_POINT('Ctrl Pts',(86.8200920815852,-1.89373933150401,-4.00759545907864));
#13183=CARTESIAN_POINT('Ctrl Pts',(86.8125431275321,-2.04381057454587,-3.93006693051597));
#13184=CARTESIAN_POINT('Ctrl Pts',(86.8087317883931,-2.11957900527457,-3.8909240885775));
#13185=CARTESIAN_POINT('Ctrl Pts',(86.8049197299082,-2.19427382669694,-3.8497037307355));
#13186=CARTESIAN_POINT('Ctrl Pts',(86.8011063358038,-2.26777209874956,-3.80645649505934));
#13187=CARTESIAN_POINT('Ctrl Pts',(86.7957167606299,-2.37164923589725,-3.74533398284062));
#13188=CARTESIAN_POINT('Ctrl Pts',(86.7904891414525,-2.47299431900228,-3.67991443977688));
#13189=CARTESIAN_POINT('Ctrl Pts',(86.7855094206065,-2.57128450374058,-3.61026854169116));
#13190=CARTESIAN_POINT('Ctrl Pts',(86.7852364479724,-2.57667246251633,-3.60645077261498));
#13191=CARTESIAN_POINT('Ctrl Pts',(86.7849642202449,-2.58205123188107,-3.60262031242433));
#13192=CARTESIAN_POINT('Ctrl Pts',(86.7846927515803,-2.58742072236894,-3.5987771758364));
#13193=CARTESIAN_POINT('Ctrl Pts',(86.7794634441658,-2.69085334677371,-3.52474674331534));
#13194=CARTESIAN_POINT('Ctrl Pts',(86.7742938009672,-2.79106535992229,-3.44632526980668));
#13195=CARTESIAN_POINT('Ctrl Pts',(86.7691194667172,-2.88765218381384,-3.36381005662206));
#13196=CARTESIAN_POINT('Ctrl Pts',(86.7639419979513,-2.98429751821472,-3.28124485724929));
#13197=CARTESIAN_POINT('Ctrl Pts',(86.7587594696479,-3.07731295376005,-3.19458071305253));
#13198=CARTESIAN_POINT('Ctrl Pts',(86.7534913658966,-3.16631392253261,-3.10415548793341));
#13199=CARTESIAN_POINT('Ctrl Pts',(86.748624450639,-3.24853708922042,-3.02061652807388));
#13200=CARTESIAN_POINT('Ctrl Pts',(86.7436840515152,-3.32733425175784,-2.93386709805201));
#13201=CARTESIAN_POINT('Ctrl Pts',(86.7385992610495,-3.40242116709039,-2.84420867629675));
#13202=CARTESIAN_POINT('Ctrl Pts',(86.7381722297014,-3.40872712343126,-2.83667897434168));
#13203=CARTESIAN_POINT('Ctrl Pts',(86.7377441799624,-3.41500694072864,-2.82912874699072));
#13204=CARTESIAN_POINT('Ctrl Pts',(86.737315069832,-3.42126046666564,-2.82155816792788));
#13205=CARTESIAN_POINT('Ctrl Pts',(86.7348897946573,-3.45660458962502,-2.77877023037616));
#13206=CARTESIAN_POINT('Ctrl Pts',(86.7324305723846,-3.49110816417236,-2.73533309406431));
#13207=CARTESIAN_POINT('Ctrl Pts',(86.7299296948,-3.52474307265858,-2.6912817437279));
#13208=CARTESIAN_POINT('Ctrl Pts',(86.7299276596136,-3.5247704443736,-2.69124589522818));
#13209=CARTESIAN_POINT('Ctrl Pts',(86.7299256243996,-3.52479781551352,-2.69121004632165));
#13210=CARTESIAN_POINT('Ctrl Pts',(86.729923589158,-3.52482518607833,-2.69117419700836));
#13211=CARTESIAN_POINT('Ctrl Pts',(86.7247422939637,-3.59450486297602,-2.59990941734138));
#13212=CARTESIAN_POINT('Ctrl Pts',(86.7193716830042,-3.66064459925158,-2.50574769312633));
#13213=CARTESIAN_POINT('Ctrl Pts',(86.7138884207033,-3.72303036313091,-2.40901285428436));
#13214=CARTESIAN_POINT('Ctrl Pts',(86.7133273451294,-3.72941399505467,-2.3991144485108));
#13215=CARTESIAN_POINT('Ctrl Pts',(86.7127650900471,-3.73575832287904,-2.38918914607351));
#13216=CARTESIAN_POINT('Ctrl Pts',(86.7122017375937,-3.74206311899499,-2.37923732457273));
#13217=CARTESIAN_POINT('Ctrl Pts',(86.7061401265042,-3.80990203906345,-2.27215680826239));
#13218=CARTESIAN_POINT('Ctrl Pts',(86.6999520037199,-3.8731643273773,-2.16200003631719));
#13219=CARTESIAN_POINT('Ctrl Pts',(86.6937289581471,-3.93161176112492,-2.04921595587832));
#13220=CARTESIAN_POINT('Ctrl Pts',(86.687511954482,-3.99000244870243,-1.93654137664771));
#13221=CARTESIAN_POINT('Ctrl Pts',(86.6812604481921,-4.04358797074338,-1.8212447305624));
#13222=CARTESIAN_POINT('Ctrl Pts',(86.6750484188064,-4.09217204731032,-1.70378344503025));
#13223=CARTESIAN_POINT('Ctrl Pts',(86.6703248143745,-4.12911520149415,-1.61446631298462));
#13224=CARTESIAN_POINT('Ctrl Pts',(86.6656241563928,-4.16316753521566,-1.52389481419493));
#13225=CARTESIAN_POINT('Ctrl Pts',(86.6610629657549,-4.19410319316702,-1.43223010271598));
#13226=CARTESIAN_POINT('Ctrl Pts',(86.659630195034,-4.2038207665952,-1.40343619227226));
#13227=CARTESIAN_POINT('Ctrl Pts',(86.6582111859304,-4.21323068902726,-1.37453477885787));
#13228=CARTESIAN_POINT('Ctrl Pts',(86.6568095500407,-4.22232567036051,-1.34553187995964));
#13229=CARTESIAN_POINT('Ctrl Pts',(86.6518979948167,-4.25419593239208,-1.24390110649319));
#13230=CARTESIAN_POINT('Ctrl Pts',(86.6471104298357,-4.28234537290711,-1.14107513937407));
#13231=CARTESIAN_POINT('Ctrl Pts',(86.6423435868528,-4.30690389679484,-1.0373873232451));
#13232=CARTESIAN_POINT('Ctrl Pts',(86.6414221494231,-4.31165109388304,-1.01734432306076));
#13233=CARTESIAN_POINT('Ctrl Pts',(86.6405014862797,-4.31626414482736,-0.997268966085684));
#13234=CARTESIAN_POINT('Ctrl Pts',(86.6395808515379,-4.32074402446021,-0.977163438477885));
#13235=CARTESIAN_POINT('Ctrl Pts',(86.6320580262991,-4.35735067206886,-0.812874210989112));
#13236=CARTESIAN_POINT('Ctrl Pts',(86.6245370168181,-4.38507002416069,-0.646569015077811));
#13237=CARTESIAN_POINT('Ctrl Pts',(86.6170124913105,-4.40373588982307,-0.479238878070492));
#13238=CARTESIAN_POINT('Ctrl Pts',(86.6131701100334,-4.41326757028192,-0.393792136626068));
#13239=CARTESIAN_POINT('Ctrl Pts',(86.6093268276084,-4.42043756843836,-0.308078337635977));
#13240=CARTESIAN_POINT('Ctrl Pts',(86.6054820079124,-4.42521857890916,-0.222230952065899));
#13241=CARTESIAN_POINT('Ctrl Pts',(86.6021218392718,-4.42939692866916,-0.14720488695166));
#13242=CARTESIAN_POINT('Ctrl Pts',(86.5987605042762,-4.4317505286615,-0.0720731711144324));
#13243=CARTESIAN_POINT('Ctrl Pts',(86.5955266375048,-4.43203607817087,0.00306014718217265));
#13244=CARTESIAN_POINT('',(85.3499542888372,-4.43459181384856,-0.00121389427323767));
#13245=CARTESIAN_POINT('Ctrl Pts',(86.595526637467,-4.43203607817194,0.00306014809321447));
#13246=CARTESIAN_POINT('Ctrl Pts',(86.5898840957589,-4.43219582861552,0.138943254598236));
#13247=CARTESIAN_POINT('Ctrl Pts',(86.5843386468504,-4.42615867458735,0.274609641975266));
#13248=CARTESIAN_POINT('Ctrl Pts',(86.5788171430829,-4.41396515084367,0.409536003282953));
#13249=CARTESIAN_POINT('Ctrl Pts',(86.578365432176,-4.41296760599,0.420574247860671));
#13250=CARTESIAN_POINT('Ctrl Pts',(86.5779138815287,-4.41192884278177,0.431607564185417));
#13251=CARTESIAN_POINT('Ctrl Pts',(86.5774624510902,-4.41084887490884,0.442635678585354));
#13252=CARTESIAN_POINT('Ctrl Pts',(86.5721566451797,-4.39815566808379,0.572252624123666));
#13253=CARTESIAN_POINT('Ctrl Pts',(86.5668669930949,-4.37977198140099,0.701148564835273));
#13254=CARTESIAN_POINT('Ctrl Pts',(86.5615075352585,-4.35575864894718,0.828850424506818));
#13255=CARTESIAN_POINT('Ctrl Pts',(86.5608048865756,-4.35261039460215,0.84559270446119));
#13256=CARTESIAN_POINT('Ctrl Pts',(86.5601010380454,-4.34936535441272,0.862314530342428));
#13257=CARTESIAN_POINT('Ctrl Pts',(86.5593957959606,-4.34602364389209,0.879014898987103));
#13258=CARTESIAN_POINT('Ctrl Pts',(86.5542953886152,-4.32185593573823,0.999794252247937));
#13259=CARTESIAN_POINT('Ctrl Pts',(86.5491214484734,-4.29263264903697,1.11944867369579));
#13260=CARTESIAN_POINT('Ctrl Pts',(86.5437895135129,-4.25843415252819,1.23756406555488));
#13261=CARTESIAN_POINT('Ctrl Pts',(86.5427220025229,-4.25158724401638,1.26121204322802));
#13262=CARTESIAN_POINT('Ctrl Pts',(86.5416481584107,-4.24454090257586,1.28479849707436));
#13263=CARTESIAN_POINT('Ctrl Pts',(86.5405673033412,-4.23729575710899,1.3083203545886));
#13264=CARTESIAN_POINT('Ctrl Pts',(86.5385206154844,-4.22357647904161,1.35286092390836));
#13265=CARTESIAN_POINT('Ctrl Pts',(86.5364487051521,-4.20914485426276,1.39716888383166));
#13266=CARTESIAN_POINT('Ctrl Pts',(86.5343468386373,-4.19400659716224,1.44122164868843));
#13267=CARTESIAN_POINT('Ctrl Pts',(86.5343448034482,-4.19399193913564,1.4412643039687));
#13268=CARTESIAN_POINT('Ctrl Pts',(86.5343427682311,-4.19397728044653,1.44130695900981));
#13269=CARTESIAN_POINT('Ctrl Pts',(86.5343407329859,-4.19396262109495,1.44134961381174));
#13270=CARTESIAN_POINT('Ctrl Pts',(86.5291554539045,-4.15661438039804,1.55002302960332));
#13271=CARTESIAN_POINT('Ctrl Pts',(86.5237807607676,-4.11488773180388,1.65734929203859));
#13272=CARTESIAN_POINT('Ctrl Pts',(86.518293531478,-4.0689351687674,1.76297028493064));
#13273=CARTESIAN_POINT('Ctrl Pts',(86.5177366776166,-4.06427182032342,1.77368889256226));
#13274=CARTESIAN_POINT('Ctrl Pts',(86.5171786647955,-4.05956498879926,1.78438991524111));
#13275=CARTESIAN_POINT('Ctrl Pts',(86.516619573361,-4.05481485937499,1.79507296354883));
#13276=CARTESIAN_POINT('Ctrl Pts',(86.5105586060111,-4.00331992031054,1.91088515991082));
#13277=CARTESIAN_POINT('Ctrl Pts',(86.5043714138943,-3.94673164378681,2.02458842439447));
#13278=CARTESIAN_POINT('Ctrl Pts',(86.4981495724106,-3.88529318864992,2.13573643973071));
#13279=CARTESIAN_POINT('Ctrl Pts',(86.4919337729579,-3.82391439640502,2.2467765192144));
#13280=CARTESIAN_POINT('Ctrl Pts',(86.4856837422683,-3.7576951524283,2.3552665180663));
#13281=CARTESIAN_POINT('Ctrl Pts',(86.4794734096533,-3.68690879741531,2.46079060385499));
#13282=CARTESIAN_POINT('Ctrl Pts',(86.4747551614893,-3.63312945735728,2.54096164378072));
#13283=CARTESIAN_POINT('Ctrl Pts',(86.4700599469391,-3.57671220342748,2.61942314447183));
#13284=CARTESIAN_POINT('Ctrl Pts',(86.4655046961467,-3.51766551356299,2.695898297196));
#13285=CARTESIAN_POINT('Ctrl Pts',(86.4640684891769,-3.49904891671944,2.72000984502505));
#13286=CARTESIAN_POINT('Ctrl Pts',(86.4626461953444,-3.48017118064383,2.74392363369086));
#13287=CARTESIAN_POINT('Ctrl Pts',(86.4612414793683,-3.46103326987111,2.76763017021447));
#13288=CARTESIAN_POINT('Ctrl Pts',(86.4563290396104,-3.39410597968449,2.85053442596512));
#13289=CARTESIAN_POINT('Ctrl Pts',(86.4515402767393,-3.3241230461927,2.93099971165257));
#13290=CARTESIAN_POINT('Ctrl Pts',(86.4467723258545,-3.2514344884534,3.00894941425027));
#13291=CARTESIAN_POINT('Ctrl Pts',(86.4458546824062,-3.23744479342866,3.02395167320996));
#13292=CARTESIAN_POINT('Ctrl Pts',(86.4449378098577,-3.22335476887946,3.03886086123303));
#13293=CARTESIAN_POINT('Ctrl Pts',(86.4440209748886,-3.20916674829457,3.05367658334066));
#13294=CARTESIAN_POINT('Ctrl Pts',(86.4364724397945,-3.09235317234639,3.17565818530495));
#13295=CARTESIAN_POINT('Ctrl Pts',(86.428926370269,-2.96889825024285,3.29130872838656));
#13296=CARTESIAN_POINT('Ctrl Pts',(86.4213774165328,-2.8395457373524,3.39993642494658));
#13297=CARTESIAN_POINT('Ctrl Pts',(86.4175660785136,-2.77423785926992,3.45478069665648));
#13298=CARTESIAN_POINT('Ctrl Pts',(86.4137540211494,-2.70742632237651,3.5078339594565));
#13299=CARTESIAN_POINT('Ctrl Pts',(86.4099406281668,-2.63920521289093,3.5590022653388));
#13300=CARTESIAN_POINT('Ctrl Pts',(86.4045511286379,-2.54278776021794,3.63131885104026));
#13301=CARTESIAN_POINT('Ctrl Pts',(86.3993235779102,-2.44338026879274,3.69964369565582));
#13302=CARTESIAN_POINT('Ctrl Pts',(86.3943439199277,-2.34124934016117,3.76352153528519));
#13303=CARTESIAN_POINT('Ctrl Pts',(86.3940708776871,-2.3356493456058,3.76702405463879));
#13304=CARTESIAN_POINT('Ctrl Pts',(86.3937985807351,-2.33004117476534,3.7705131983715));
#13305=CARTESIAN_POINT('Ctrl Pts',(86.3935270432396,-2.32442487571878,3.77398888953018));
#13306=CARTESIAN_POINT('Ctrl Pts',(86.3882977366634,-2.21626541332121,3.84092422970094));
#13307=CARTESIAN_POINT('Ctrl Pts',(86.3831280944019,-2.10529429770412,3.90319607655686));
#13308=CARTESIAN_POINT('Ctrl Pts',(86.3779537612096,-1.99194172975216,3.96054558939924));
#13309=CARTESIAN_POINT('Ctrl Pts',(86.3727762935036,-1.87852049494594,4.01792984349814));
#13310=CARTESIAN_POINT('Ctrl Pts',(86.3675937663811,-1.76271481841343,4.0703854124142));
#13311=CARTESIAN_POINT('Ctrl Pts',(86.3623256639482,-1.64498462590344,4.11768754589881));
#13312=CARTESIAN_POINT('Ctrl Pts',(86.3574587493474,-1.53622007544583,4.16138742589096));
#13313=CARTESIAN_POINT('Ctrl Pts',(86.3525183509811,-1.42581246032295,4.200689015183));
#13314=CARTESIAN_POINT('Ctrl Pts',(86.3474335613535,-1.31414948416729,4.23544613142731));
#13315=CARTESIAN_POINT('Ctrl Pts',(86.3470065307072,-1.30477180753288,4.23836510249637));
#13316=CARTESIAN_POINT('Ctrl Pts',(86.3465784816734,-1.29538525792704,4.24125204537026));
#13317=CARTESIAN_POINT('Ctrl Pts',(86.3461493722522,-1.28599005430222,4.24410688638762));
#13318=CARTESIAN_POINT('Ctrl Pts',(86.3437240899407,-1.23288932978963,4.26024215417355));
#13319=CARTESIAN_POINT('Ctrl Pts',(86.3412648603392,-1.17951327293067,4.27535166039204));
#13320=CARTESIAN_POINT('Ctrl Pts',(86.3387639751587,-1.12590500003043,4.28942293282578));
#13321=CARTESIAN_POINT('Ctrl Pts',(86.3387619399709,-1.12586137431477,4.28943438384438));
#13322=CARTESIAN_POINT('Ctrl Pts',(86.3387599047554,-1.12581774844521,4.28944583417556));
#13323=CARTESIAN_POINT('Ctrl Pts',(86.3387578695124,-1.12577412242181,4.28945728381933));
#13324=CARTESIAN_POINT('Ctrl Pts',(86.3335725900635,-1.01462615662874,4.31862805197162));
#13325=CARTESIAN_POINT('Ctrl Pts',(86.3281978965953,-0.902171760511038,
4.34340808868859));
#13326=CARTESIAN_POINT('Ctrl Pts',(86.3227106670089,-0.788793515388748,
4.36372574881666));
#13327=CARTESIAN_POINT('Ctrl Pts',(86.3221538132375,-0.777287690382657,
4.36578762093079));
#13328=CARTESIAN_POINT('Ctrl Pts',(86.3215958005074,-0.765772391249227,
4.36780355560554));
#13329=CARTESIAN_POINT('Ctrl Pts',(86.3210367091646,-0.754248044742652,
4.36977349104319));
#13330=CARTESIAN_POINT('Ctrl Pts',(86.3149757416187,-0.629315525087442,
4.39112906184654));
#13331=CARTESIAN_POINT('Ctrl Pts',(86.3087885493506,-0.503314160078422,
4.40707655958354));
#13332=CARTESIAN_POINT('Ctrl Pts',(86.3025667077508,-0.376750202562136,
4.4175708908222));
#13333=CARTESIAN_POINT('Ctrl Pts',(86.2963509081796,-0.250309151268211,
4.42805503101884));
#13334=CARTESIAN_POINT('Ctrl Pts',(86.2901008774065,-0.123306599074165,
4.43309696528657));
#13335=CARTESIAN_POINT('Ctrl Pts',(86.2838905447321,0.00375983736620393,
4.43269362025351));
#13336=CARTESIAN_POINT('Ctrl Pts',(86.2791722989182,0.100297448676526,4.43238718240008));
#13337=CARTESIAN_POINT('Ctrl Pts',(86.2744770867086,0.196874904896678,4.42893757612002));
#13338=CARTESIAN_POINT('Ctrl Pts',(86.2699218382983,0.293257138992177,4.42219838301227));
#13339=CARTESIAN_POINT('Ctrl Pts',(86.2684856290359,0.323645176014095,4.42007360502202));
#13340=CARTESIAN_POINT('Ctrl Pts',(86.2670633329739,0.354013419053023,4.41762185408007));
#13341=CARTESIAN_POINT('Ctrl Pts',(86.2656586148563,0.384353433004181,4.41483866957661));
#13342=CARTESIAN_POINT('Ctrl Pts',(86.2607461705137,0.490455595436704,4.40510558590888));
#13343=CARTESIAN_POINT('Ctrl Pts',(86.2559574027941,0.596222158195863,4.39147725368983));
#13344=CARTESIAN_POINT('Ctrl Pts',(86.251189446914,0.701395296850439,4.37420248981706));
#13345=CARTESIAN_POINT('Ctrl Pts',(86.2502718083016,0.72163687111139,4.37087779664689));
#13346=CARTESIAN_POINT('Ctrl Pts',(86.2493549405738,0.741856616416203,4.36741800606075));
#13347=CARTESIAN_POINT('Ctrl Pts',(86.2484381104248,0.762052910300203,4.36382484101895));
#13348=CARTESIAN_POINT('Ctrl Pts',(86.2408895753065,0.928335000633039,4.33424124526154));
#13349=CARTESIAN_POINT('Ctrl Pts',(86.2333435057538,1.09303045899132,4.29562037199433));
#13350=CARTESIAN_POINT('Ctrl Pts',(86.2257945519879,1.25515119566418,4.24819763754719));
#13351=CARTESIAN_POINT('Ctrl Pts',(86.2219832135279,1.33700320032816,4.22425470488596));
#13352=CARTESIAN_POINT('Ctrl Pts',(86.218171155722,1.41819837270992,4.19806738441553));
#13353=CARTESIAN_POINT('Ctrl Pts',(86.2143577622969,1.4986063618513,4.16966188842326));
#13354=CARTESIAN_POINT('Ctrl Pts',(86.2089682434684,1.6122480250964,4.12951602923274));
#13355=CARTESIAN_POINT('Ctrl Pts',(86.203740675327,1.72422545010329,4.08466857362693));
#13356=CARTESIAN_POINT('Ctrl Pts',(86.1987610014044,1.83401193600097,4.03508897922655));
#13357=CARTESIAN_POINT('Ctrl Pts',(86.1984879768791,1.84003128659781,4.03237063954472));
#13358=CARTESIAN_POINT('Ctrl Pts',(86.1982156975453,1.84604403978771,4.0296380812244));
#13359=CARTESIAN_POINT('Ctrl Pts',(86.197944177568,1.85205010488924,4.02689130161306));
#13360=CARTESIAN_POINT('Ctrl Pts',(86.1927148708447,1.96772320168933,3.97399002623559));
#13361=CARTESIAN_POINT('Ctrl Pts',(86.1875452283948,2.08107412016809,3.91616319949736));
#13362=CARTESIAN_POINT('Ctrl Pts',(86.182370894962,2.19164892640812,3.85362533328131));
#13363=CARTESIAN_POINT('Ctrl Pts',(86.1771934270152,2.30229071678806,3.791049582801));
#13364=CARTESIAN_POINT('Ctrl Pts',(86.1720108995998,2.41015276677152,3.72375678365849));
#13365=CARTESIAN_POINT('Ctrl Pts',(86.1667427968143,2.51479303267953,3.65200508658382));
#13366=CARTESIAN_POINT('Ctrl Pts',(86.1618758821495,2.61146450349588,3.58571758215531));
#13367=CARTESIAN_POINT('Ctrl Pts',(86.1569354836762,2.70538659224564,3.51562409301069));
#13368=CARTESIAN_POINT('Ctrl Pts',(86.1518506939089,2.79622268420564,3.44196622604107));
#13369=CARTESIAN_POINT('Ctrl Pts',(86.1514236629565,2.80385128334945,3.43578028905529));
#13370=CARTESIAN_POINT('Ctrl Pts',(86.150995613615,2.81145814736353,3.42956921003236));
#13371=CARTESIAN_POINT('Ctrl Pts',(86.1505665038843,2.81904309354882,3.42333313034923));
#13372=CARTESIAN_POINT('Ctrl Pts',(86.1481412239167,2.86191235687148,3.38808750888977));
#13373=CARTESIAN_POINT('Ctrl Pts',(86.1456819967187,2.90408061354856,3.35204402790925));
#13374=CARTESIAN_POINT('Ctrl Pts',(86.1431811140263,2.94551357861408,3.31523165464269));
#13375=CARTESIAN_POINT('Ctrl Pts',(86.1431790788384,2.94554729625724,3.31520169718095));
#13376=CARTESIAN_POINT('Ctrl Pts',(86.1431770436228,2.94558101341364,3.31517173921001));
#13377=CARTESIAN_POINT('Ctrl Pts',(86.1431750083797,2.94561473008326,3.3151417807299));
#13378=CARTESIAN_POINT('Ctrl Pts',(86.1379897289487,3.03151618984276,3.23881522763576));
#13379=CARTESIAN_POINT('Ctrl Pts',(86.1326150355066,3.11448791527129,3.15896703602293));
#13380=CARTESIAN_POINT('Ctrl Pts',(86.1271278059603,3.19425816325917,3.0758758762552));
#13381=CARTESIAN_POINT('Ctrl Pts',(86.1265709523188,3.20235338739831,3.0674436401864));
#13382=CARTESIAN_POINT('Ctrl Pts',(86.1260129397191,3.21041563415425,3.05897804999534));
#13383=CARTESIAN_POINT('Ctrl Pts',(86.1254538485075,3.21844461548815,3.05047942657368));
#13384=CARTESIAN_POINT('Ctrl Pts',(86.1193928811413,3.30548478502846,2.95834798514696));
#13385=CARTESIAN_POINT('Ctrl Pts',(86.1132056890736,3.38861683791079,2.86232857457603));
#13386=CARTESIAN_POINT('Ctrl Pts',(86.1069838476934,3.46752255960513,2.76281750892179));
#13387=CARTESIAN_POINT('Ctrl Pts',(86.1007680483423,3.54635165596562,2.66340307844765));
#13388=CARTESIAN_POINT('Ctrl Pts',(86.0945180178085,3.62096293755536,2.56050397832784));
#13389=CARTESIAN_POINT('Ctrl Pts',(86.0883076853898,3.69107794818618,2.45453263297218));
#13390=CARTESIAN_POINT('Ctrl Pts',(86.0835894400834,3.74434720939639,2.37402183755535));
#13391=CARTESIAN_POINT('Ctrl Pts',(86.0788942283879,3.79502274304321,2.29173518500281));
#13392=CARTESIAN_POINT('Ctrl Pts',(86.0743389805092,3.84285236572728,2.20778712345346));
#13393=CARTESIAN_POINT('Ctrl Pts',(86.0729027710171,3.85793241404427,2.18131940840073));
#13394=CARTESIAN_POINT('Ctrl Pts',(86.0714804747347,3.87272937300033,2.15468687949912));
#13395=CARTESIAN_POINT('Ctrl Pts',(86.0700757564095,3.88723485360502,2.1278940835062));
#13396=CARTESIAN_POINT('Ctrl Pts',(86.0651633114149,3.93796201670671,2.03419691004993));
#13397=CARTESIAN_POINT('Ctrl Pts',(86.0603745429983,3.98526139034097,1.93861934937803));
#13398=CARTESIAN_POINT('Ctrl Pts',(86.0556065863939,4.02919709767552,1.84151392321606));
#13399=CARTESIAN_POINT('Ctrl Pts',(86.0546889487526,4.03765293362169,1.82282507983735));
#13400=CARTESIAN_POINT('Ctrl Pts',(86.0537720819931,4.04598423569971,1.80407949977676));
#13401=CARTESIAN_POINT('Ctrl Pts',(86.0528552528123,4.0541915382368,1.78527948855819));
#13402=CARTESIAN_POINT('Ctrl Pts',(86.0453067179233,4.1217647687229,1.6304932496601));
#13403=CARTESIAN_POINT('Ctrl Pts',(86.0377606485988,4.18093727000537,1.47201681774839));
#13404=CARTESIAN_POINT('Ctrl Pts',(86.0302116950601,4.2313571249296,1.31080302876705));
#13405=CARTESIAN_POINT('Ctrl Pts',(86.0264003568354,4.25681325197743,1.22940892915413));
#13406=CARTESIAN_POINT('Ctrl Pts',(86.0225882992646,4.28003737230099,1.14731708322164));
#13407=CARTESIAN_POINT('Ctrl Pts',(86.0187749060743,4.30097902863963,1.06465050526195));
#13408=CARTESIAN_POINT('Ctrl Pts',(86.0133853695236,4.33057624472483,0.947816357507269));
#13409=CARTESIAN_POINT('Ctrl Pts',(86.0081577854476,4.35533792725017,0.829760468080612));
#13410=CARTESIAN_POINT('Ctrl Pts',(86.0031780969979,4.37494663312993,0.710904240823791));
#13411=CARTESIAN_POINT('Ctrl Pts',(86.0029050891604,4.37602166632583,0.704388033654169));
#13412=CARTESIAN_POINT('Ctrl Pts',(86.0026328264232,4.37708121044841,0.69786943392072));
#13413=CARTESIAN_POINT('Ctrl Pts',(86.0023613229485,4.37812521302266,0.691348515606644));
#13414=CARTESIAN_POINT('Ctrl Pts',(85.9971320165779,4.39823327727006,0.565752039462315));
#13415=CARTESIAN_POINT('Ctrl Pts',(85.9919623744859,4.41295467258498,0.439357213929078));
#13416=CARTESIAN_POINT('Ctrl Pts',(85.9867880414143,4.42221624186131,0.312660747524827));
#13417=CARTESIAN_POINT('Ctrl Pts',(85.9816105738279,4.43148342162433,0.185887530753862));
#13418=CARTESIAN_POINT('Ctrl Pts',(85.9764280467761,4.43528376276548,0.0588123608202801));
#13419=CARTESIAN_POINT('Ctrl Pts',(85.971159944355,4.43358701788811,-0.0680537539876058));
#13420=CARTESIAN_POINT('Ctrl Pts',(85.966293029979,4.43201948723363,-0.185258483248564));
#13421=CARTESIAN_POINT('Ctrl Pts',(85.9613526317935,4.42576015882048,-0.302285300534199));
#13422=CARTESIAN_POINT('Ctrl Pts',(85.9562678423078,4.41482347107894,-0.418720110591728));
#13423=CARTESIAN_POINT('Ctrl Pts',(85.9558408114293,4.41390498597982,-0.428498540824374));
#13424=CARTESIAN_POINT('Ctrl Pts',(85.9554127621619,4.412953526267,-0.438272822310485));
#13425=CARTESIAN_POINT('Ctrl Pts',(85.9549836525054,4.41196910830211,-0.448042724618684));
#13426=CARTESIAN_POINT('Ctrl Pts',(85.9525583701489,4.40640528216577,-0.503261178314962));
#13427=CARTESIAN_POINT('Ctrl Pts',(85.95009914049,4.39978879021105,-0.558338602336901));
#13428=CARTESIAN_POINT('Ctrl Pts',(85.9475982552398,4.39212473073041,-0.613230403193613));
#13429=CARTESIAN_POINT('Ctrl Pts',(85.9475962200502,4.39211849381327,-0.613275073464575));
#13430=CARTESIAN_POINT('Ctrl Pts',(85.947594184833,4.39211225620248,-0.61331974361277));
#13431=CARTESIAN_POINT('Ctrl Pts',(85.9475921495882,4.39210601789805,-0.613364413638149));
#13432=CARTESIAN_POINT('Ctrl Pts',(85.9424068704086,4.37621242585401,-0.727172126655377));
#13433=CARTESIAN_POINT('Ctrl Pts',(85.93703217718,4.35576368154846,-0.840494181412317));
#13434=CARTESIAN_POINT('Ctrl Pts',(85.9315449478011,4.33084103589823,-0.952949920937747));
#13435=CARTESIAN_POINT('Ctrl Pts',(85.9309880938758,4.32831184090763,-0.964362132027367));
#13436=CARTESIAN_POINT('Ctrl Pts',(85.9304300809907,4.32573660380383,-0.975765391395718));
#13437=CARTESIAN_POINT('Ctrl Pts',(85.9298709894921,4.32311543194047,-0.987159281414365));
#13438=CARTESIAN_POINT('Ctrl Pts',(85.9238100219872,4.29469998021658,-1.11067752006864));
#13439=CARTESIAN_POINT('Ctrl Pts',(85.9176228297165,4.26088205263452,-1.23309897558197));
#13440=CARTESIAN_POINT('Ctrl Pts',(85.9114009880802,4.22181504041481,-1.35393908995992));
#13441=CARTESIAN_POINT('Ctrl Pts',(85.9051851884749,4.18278596617458,-1.47466185649065));
#13442=CARTESIAN_POINT('Ctrl Pts',(85.8989351576339,4.13851834258754,-1.59380649644786));
#13443=CARTESIAN_POINT('Ctrl Pts',(85.8927248248716,4.08920101189957,-1.71091260746274));
#13444=CARTESIAN_POINT('Ctrl Pts',(85.8880065829692,4.05173263378374,-1.79988287381678));
#13445=CARTESIAN_POINT('Ctrl Pts',(85.8833113746208,4.01134828387334,-1.88767918590884));
#13446=CARTESIAN_POINT('Ctrl Pts',(85.8787561301198,3.96800338770175,-1.97402821645276));
#13447=CARTESIAN_POINT('Ctrl Pts',(85.8773199170399,3.95433727014978,-2.00125301351398));
#13448=CARTESIAN_POINT('Ctrl Pts',(85.875897617263,3.9403770330886,-2.0283335954952));
#13449=CARTESIAN_POINT('Ctrl Pts',(85.8744928955748,3.92612180922687,-2.05526045989324));
#13450=CARTESIAN_POINT('Ctrl Pts',(85.8695804485481,3.87626991851789,-2.14942629791357));
#13451=CARTESIAN_POINT('Ctrl Pts',(85.8647916779767,3.82295261903395,-2.24178200764895));
#13452=CARTESIAN_POINT('Ctrl Pts',(85.8600237191508,3.76649884035913,-2.33218550156041));
#13453=CARTESIAN_POINT('Ctrl Pts',(85.8591060838274,3.75563381753786,-2.34958444362464));
#13454=CARTESIAN_POINT('Ctrl Pts',(85.8581892193786,3.74465253116239,-2.36691120306815));
#13455=CARTESIAN_POINT('Ctrl Pts',(85.8572723925084,3.73355719617822,-2.38416494630189));
#13456=CARTESIAN_POINT('Ctrl Pts',(85.8497238572283,3.64220567682109,-2.52622065361032));
#13457=CARTESIAN_POINT('Ctrl Pts',(85.8421777875189,3.5431253917475,-2.66333106288721));
#13458=CARTESIAN_POINT('Ctrl Pts',(85.8346288336008,3.43691419708384,-2.79467501010445));
#13459=CARTESIAN_POINT('Ctrl Pts',(85.8308174959047,3.38328998181449,-2.86098832220123));
#13460=CARTESIAN_POINT('Ctrl Pts',(85.8270054388642,3.32784757267642,-2.92583096377285));
#13461=CARTESIAN_POINT('Ctrl Pts',(85.823192046206,3.27066136956487,-2.98909273912823));
#13462=CARTESIAN_POINT('Ctrl Pts',(85.8178026498303,3.18984118045341,-3.07849942062754));
#13463=CARTESIAN_POINT('Ctrl Pts',(85.8125751922913,3.10532341564083,-3.16455941835129));
#13464=CARTESIAN_POINT('Ctrl Pts',(85.8075956197331,3.01728274818844,-3.24677493312333));
#13465=CARTESIAN_POINT('Ctrl Pts',(85.8073224817074,3.01245356781049,-3.25128459396744));
#13466=CARTESIAN_POINT('Ctrl Pts',(85.8070500894955,3.00761379846055,-3.25578268002325));
#13467=CARTESIAN_POINT('Ctrl Pts',(85.8067784572813,3.00276347265943,-3.26026910647789));
#13468=CARTESIAN_POINT('Ctrl Pts',(85.8015491507576,2.90938780132206,-3.3466391977428));
#13469=CARTESIAN_POINT('Ctrl Pts',(85.7963795085898,2.81236114119968,-3.42896901143191));
#13470=CARTESIAN_POINT('Ctrl Pts',(85.7912051755409,2.71205630374664,-3.50692226952133));
#13471=CARTESIAN_POINT('Ctrl Pts',(85.7860277079776,2.61169070349584,-3.58492275023904));
#13472=CARTESIAN_POINT('Ctrl Pts',(85.7808451810478,2.50804277796375,-3.6585410124661));
#13473=CARTESIAN_POINT('Ctrl Pts',(85.7755770788642,2.40152103005734,-3.72746856029959));
#13474=CARTESIAN_POINT('Ctrl Pts',(85.7707101643231,2.30311135124782,-3.79114699195077));
#13475=CARTESIAN_POINT('Ctrl Pts',(85.7657697660599,2.20224841543128,-3.85082215564701));
#13476=CARTESIAN_POINT('Ctrl Pts',(85.7606849765742,2.099284847855,-3.90627647648126));
#13477=CARTESIAN_POINT('Ctrl Pts',(85.7602579461313,2.0906377685623,-3.91093363746222));
#13478=CARTESIAN_POINT('Ctrl Pts',(85.7598298973021,2.08197585954655,-3.91556105601013));
#13479=CARTESIAN_POINT('Ctrl Pts',(85.7594007880867,2.07329932164923,-3.92015861798155));
#13480=CARTESIAN_POINT('Ctrl Pts',(85.7569755051691,2.02426038612856,-3.94614358430527));
#13481=CARTESIAN_POINT('Ctrl Pts',(85.7545162749515,1.97475517878424,-3.97117430399793));
#13482=CARTESIAN_POINT('Ctrl Pts',(85.7520153891379,1.92482363811476,-3.99523029555697));
#13483=CARTESIAN_POINT('Ctrl Pts',(85.7520133539521,1.9247830045265,-3.99524987198587));
#13484=CARTESIAN_POINT('Ctrl Pts',(85.7520113187387,1.92474237065582,-3.99526944776944));
#13485=CARTESIAN_POINT('Ctrl Pts',(85.7520092834976,1.92470173650278,-3.99528902290766));
#13486=CARTESIAN_POINT('Ctrl Pts',(85.7468240038619,1.82117618607677,-4.04516152687214));
#13487=CARTESIAN_POINT('Ctrl Pts',(85.7414493102135,1.71552925404483,-4.09097385477383));
#13488=CARTESIAN_POINT('Ctrl Pts',(85.7359620804535,1.60812278109484,-4.13258257419633));
#13489=CARTESIAN_POINT('Ctrl Pts',(85.7354052266776,1.59722298235525,-4.13680510059591));
#13490=CARTESIAN_POINT('Ctrl Pts',(85.734847213943,1.58630510588221,-4.14098434647469));
#13491=CARTESIAN_POINT('Ctrl Pts',(85.7342881225959,1.57536955875698,-4.14512016962523));
#13492=CARTESIAN_POINT('Ctrl Pts',(85.7282271548735,1.45682006142753,-4.18995558114381));
#13493=CARTESIAN_POINT('Ctrl Pts',(85.7220399624372,1.3361879854999,-4.22968682176168));
#13494=CARTESIAN_POINT('Ctrl Pts',(85.7158181206739,1.21396163801592,-4.26417288909974));
#13495=CARTESIAN_POINT('Ctrl Pts',(85.7096023209395,1.09185398450512,-4.29862546702709));
#13496=CARTESIAN_POINT('Ctrl Pts',(85.7033522900078,0.968155225385933,-4.32784342167491));
#13497=CARTESIAN_POINT('Ctrl Pts',(85.6971419571728,0.843353220264177,-4.35172864669007));
#13498=CARTESIAN_POINT('Ctrl Pts',(85.6924237080598,0.748535926953768,-4.36987524925338));
#13499=CARTESIAN_POINT('Ctrl Pts',(85.687728492581,0.653078893740779,-4.38494421345017));
#13500=CARTESIAN_POINT('Ctrl Pts',(85.6831732408483,0.557184877352213,-4.39674690018236));
#13501=CARTESIAN_POINT('Ctrl Pts',(85.6817370345738,0.526950853830489,-4.4004681199385));
#13502=CARTESIAN_POINT('Ctrl Pts',(85.6803147414161,0.496673778449594,-4.40386461098195));
#13503=CARTESIAN_POINT('Ctrl Pts',(85.6789100260858,0.466361078450329,-4.40693038309136));
#13504=CARTESIAN_POINT('Ctrl Pts',(85.6739975838905,0.360354271715672,-4.41765172139186));
#13505=CARTESIAN_POINT('Ctrl Pts',(85.6692088184592,0.253932537364538,-4.42448546452957));
#13506=CARTESIAN_POINT('Ctrl Pts',(85.6644408649485,0.147396494829036,-4.42762657668275));
#13507=CARTESIAN_POINT('Ctrl Pts',(85.6635232234467,0.126892541960029,-4.42823111589795));
#13508=CARTESIAN_POINT('Ctrl Pts',(85.6626063528382,0.106384199984283,-4.42869887504062));
#13509=CARTESIAN_POINT('Ctrl Pts',(85.6616895198087,0.0858733907272211,
-4.42903123529975));
#13510=CARTESIAN_POINT('Ctrl Pts',(85.6541409846172,-0.0829976692238332,
-4.43176764752723));
#13511=CARTESIAN_POINT('Ctrl Pts',(85.6465949149874,-0.252038268960491,
-4.42533012680183));
#13512=CARTESIAN_POINT('Ctrl Pts',(85.6390459611412,-0.420233541092514,
-4.40976093706903));
#13513=CARTESIAN_POINT('Ctrl Pts',(85.6352346217969,-0.505152494272502,
-4.40190031603486));
#13514=CARTESIAN_POINT('Ctrl Pts',(85.6314225631056,-0.589855599106871,
-4.39171115039403));
#13515=CARTESIAN_POINT('Ctrl Pts',(85.6276091687937,-0.674209897682507,
-4.37919426061962));
#13516=CARTESIAN_POINT('Ctrl Pts',(85.6222195647431,-0.793430789127758,
-4.36150370089445));
#13517=CARTESIAN_POINT('Ctrl Pts',(85.6169919195691,-0.911916514284298,
-4.33888000264703));
#13518=CARTESIAN_POINT('Ctrl Pts',(85.6120121749869,-1.02915589167847,-4.31119254294835));
#13519=CARTESIAN_POINT('Ctrl Pts',(85.611739229202,-1.03558192284624,-4.30967496000878));
#13520=CARTESIAN_POINT('Ctrl Pts',(85.6114670281768,-1.04200419735488,-4.30814216848057));
#13521=CARTESIAN_POINT('Ctrl Pts',(85.6111955860632,-1.04842262677744,-4.30659414845052));
#13522=CARTESIAN_POINT('Ctrl Pts',(85.6059662788624,-1.17207307566988,-4.27677168581844));
#13523=CARTESIAN_POINT('Ctrl Pts',(85.6007966358639,-1.29438536193029,-4.2416706913012));
#13524=CARTESIAN_POINT('Ctrl Pts',(85.5956223017994,-1.4148729253243,-4.20141498159159));
#13525=CARTESIAN_POINT('Ctrl Pts',(85.5904448332242,-1.53543347773565,-4.16113488575772));
#13526=CARTESIAN_POINT('Ctrl Pts',(85.5852623050967,-1.65416689427829,-4.11569348298227));
#13527=CARTESIAN_POINT('Ctrl Pts',(85.57999420151,-1.77058994689207,-4.06525969676661));
#13528=CARTESIAN_POINT('Ctrl Pts',(85.575127286506,-1.87814688692753,-4.01866665872152));
#13529=CARTESIAN_POINT('Ctrl Pts',(85.5701868876291,-1.98373239500671,-3.96781239106193));
#13530=CARTESIAN_POINT('Ctrl Pts',(85.5651020974149,-2.08696989070404,-3.91286972470537));
#13531=CARTESIAN_POINT('Ctrl Pts',(85.5646750659807,-2.09563999389301,-3.90825552340602));
#13532=CARTESIAN_POINT('Ctrl Pts',(85.564247016155,-2.10429356683553,-3.90361248994626));
#13533=CARTESIAN_POINT('Ctrl Pts',(85.5638179059376,-2.11293040318291,-3.89894072818614));
#13534=CARTESIAN_POINT('Ctrl Pts',(85.5613926308205,-2.16174467847522,-3.87253653856314));
#13535=CARTESIAN_POINT('Ctrl Pts',(85.5589334086046,-2.21002333018883,-3.84521524038816));
#13536=CARTESIAN_POINT('Ctrl Pts',(85.5564325310774,-2.2577271700392,-3.81699871544304));
#13537=CARTESIAN_POINT('Ctrl Pts',(85.556430495889,-2.25776599093189,-3.81697575312616));
#13538=CARTESIAN_POINT('Ctrl Pts',(85.5564284606731,-2.25780481144409,-3.81695279021645));
#13539=CARTESIAN_POINT('Ctrl Pts',(85.5564264254296,-2.25784363157577,-3.81692982671393));
#13540=CARTESIAN_POINT('Ctrl Pts',(85.551241145975,-2.35674738960827,-3.75842470068692));
#13541=CARTESIAN_POINT('Ctrl Pts',(85.5458664525601,-2.45344835146911,-3.69590298795353));
#13542=CARTESIAN_POINT('Ctrl Pts',(85.5403792231113,-2.54762653041449,-3.62958629625731));
#13543=CARTESIAN_POINT('Ctrl Pts',(85.5398223700601,-2.55718388659679,-3.62285636953257));
#13544=CARTESIAN_POINT('Ctrl Pts',(85.539264358054,-2.56671524678532,-3.61608740174902));
#13545=CARTESIAN_POINT('Ctrl Pts',(85.5387052674388,-2.57622026693092,-3.60927965284289));
#13546=CARTESIAN_POINT('Ctrl Pts',(85.5326443008004,-2.67926189996543,-3.53547848737126));
#13547=CARTESIAN_POINT('Ctrl Pts',(85.5264571095619,-2.77921038643425,-3.45711419679469));
#13548=CARTESIAN_POINT('Ctrl Pts',(85.5202352690982,-2.87567764407725,-3.37451498435399));
#13549=CARTESIAN_POINT('Ctrl Pts',(85.5140194706598,-2.97205122242823,-3.2919959839555));
#13550=CARTESIAN_POINT('Ctrl Pts',(85.5077694411254,-3.06495059658092,-3.20525054580355));
#13551=CARTESIAN_POINT('Ctrl Pts',(85.501559109773,-3.1540236314308,-3.11463028404254));
#13552=CARTESIAN_POINT('Ctrl Pts',(85.4968408579376,-3.22169618967374,-3.04578223196543));
#13553=CARTESIAN_POINT('Ctrl Pts',(85.4921456398231,-3.28716215867454,-2.97469540514654));
#13554=CARTESIAN_POINT('Ctrl Pts',(85.4875903854759,-3.35015213193905,-2.90143395399441));
#13555=CARTESIAN_POINT('Ctrl Pts',(85.4861541832599,-3.37001190974662,-2.87833573587593));
#13556=CARTESIAN_POINT('Ctrl Pts',(85.4847318940682,-3.38962531165613,-2.85502164769157));
#13557=CARTESIAN_POINT('Ctrl Pts',(85.483327182572,-3.40898323459362,-2.83149454933526));
#13558=CARTESIAN_POINT('Ctrl Pts',(85.4784147446847,-3.47668012062022,-2.74921757669169));
#13559=CARTESIAN_POINT('Ctrl Pts',(85.4736259837766,-3.54137171508201,-2.66443985809102));
#13560=CARTESIAN_POINT('Ctrl Pts',(85.468858034897,-3.60305359689301,-2.57751967162226));
#13561=CARTESIAN_POINT('Ctrl Pts',(85.4679403901104,-3.61492496101744,-2.56079091508893));
#13562=CARTESIAN_POINT('Ctrl Pts',(85.4670235162279,-3.62668492620405,-2.54398266893432));
#13563=CARTESIAN_POINT('Ctrl Pts',(85.4661066799248,-3.63833357637928,-2.52709729836248));
#13564=CARTESIAN_POINT('Ctrl Pts',(85.4585581460186,-3.73423971633857,-2.3880759792425));
#13565=CARTESIAN_POINT('Ctrl Pts',(85.4510120776706,-3.82260509299389,-2.24382717287147));
#13566=CARTESIAN_POINT('Ctrl Pts',(85.4434631251022,-3.9029021966404,-2.09521890865093));
#13567=CARTESIAN_POINT('Ctrl Pts',(85.4396517872357,-3.94344283971919,-2.02018912146399));
#13568=CARTESIAN_POINT('Ctrl Pts',(85.4358397300216,-3.98192593919025,-1.94404793137696));
#13569=CARTESIAN_POINT('Ctrl Pts',(85.4320263371865,-4.01827846077401,-1.86690644393239));
#13570=CARTESIAN_POINT('Ctrl Pts',(85.4266365949618,-4.06965809277716,-1.75787683430971));
#13571=CARTESIAN_POINT('Ctrl Pts',(85.4214088253351,-4.11652440392096,-1.64672380638182));
#13572=CARTESIAN_POINT('Ctrl Pts',(85.4164289670649,-4.15848525213285,-1.5338003894688));
#13573=CARTESIAN_POINT('Ctrl Pts',(85.4161561509682,-4.16078403137511,-1.52761400340116));
#13574=CARTESIAN_POINT('Ctrl Pts',(85.4158840789221,-4.16306808473654,-1.52142231651565));
#13575=CARTESIAN_POINT('Ctrl Pts',(85.4156127650568,-4.16533734671304,-1.51522539127473));
#13576=CARTESIAN_POINT('Ctrl Pts',(85.4103834597761,-4.20907511743536,-1.39578581216136));
#13577=CARTESIAN_POINT('Ctrl Pts',(85.4052138187203,-4.24767803984522,-1.27453325637026));
#13578=CARTESIAN_POINT('Ctrl Pts',(85.4000394866055,-4.28097938890212,-1.1519412996419));
#13579=CARTESIAN_POINT('Ctrl Pts',(85.3948620199694,-4.31430091134194,-1.02927507882045));
#13580=CARTESIAN_POINT('Ctrl Pts',(85.3896794937884,-4.34231403673318,-0.905267810486362));
#13581=CARTESIAN_POINT('Ctrl Pts',(85.3844113921312,-4.36489142648191,-0.780415306259535));
#13582=CARTESIAN_POINT('Ctrl Pts',(85.3795444786099,-4.38574945288143,-0.665070846240425));
#13583=CARTESIAN_POINT('Ctrl Pts',(85.3746040811925,-4.40196814370703,-0.549004463717536));
#13584=CARTESIAN_POINT('Ctrl Pts',(85.3695192923719,-4.41348254186089,-0.432625382137005));
#13585=CARTESIAN_POINT('Ctrl Pts',(85.3690922613637,-4.414449544666,-0.422851627847718));
#13586=CARTESIAN_POINT('Ctrl Pts',(85.368664211965,-4.41538338769334,-0.413075644729704));
#13587=CARTESIAN_POINT('Ctrl Pts',(85.3682351021756,-4.41628404296986,-0.403297662094833));
#13588=CARTESIAN_POINT('Ctrl Pts',(85.3658098126881,-4.42137446464771,-0.34803339388098));
#13589=CARTESIAN_POINT('Ctrl Pts',(85.363350575666,-4.42540466293366,-0.292706402114392));
#13590=CARTESIAN_POINT('Ctrl Pts',(85.3608496827478,-4.42837112077165,-0.237361433173412));
#13591=CARTESIAN_POINT('Ctrl Pts',(85.36084764755,-4.42837353484072,-0.237316394077848));
#13592=CARTESIAN_POINT('Ctrl Pts',(85.3608456123247,-4.42837594820546,-0.237271354970261));
#13593=CARTESIAN_POINT('Ctrl Pts',(85.3608435770718,-4.42837836086587,-0.237226315850657));
#13594=CARTESIAN_POINT('Ctrl Pts',(85.3572923046138,-4.43258816420395,-0.158638448753409));
#13595=CARTESIAN_POINT('Ctrl Pts',(85.3536546163276,-4.4346561875942,-0.0799395109034866));
#13596=CARTESIAN_POINT('Ctrl Pts',(85.3499542888701,-4.43459181384913,-0.00121389497252961));
#13597=CARTESIAN_POINT('',(84.0953986853364,-4.42975181744819,-0.00129412797191142));
#13598=CARTESIAN_POINT('Ctrl Pts',(85.3499542888372,-4.43459181384856,-0.00121389427323007));
#13599=CARTESIAN_POINT('Ctrl Pts',(85.3443627450434,-4.43449453902907,0.117747936589198));
#13600=CARTESIAN_POINT('Ctrl Pts',(85.3386250062462,-4.42952256215798,0.236873214595778));
#13601=CARTESIAN_POINT('Ctrl Pts',(85.3328212751709,-4.41970267314065,0.355734616697525));
#13602=CARTESIAN_POINT('Ctrl Pts',(85.3324982112812,-4.41915605037309,0.362351020249405));
#13603=CARTESIAN_POINT('Ctrl Pts',(85.3321749429093,-4.41859441338435,0.368966594981758));
#13604=CARTESIAN_POINT('Ctrl Pts',(85.3318514838888,-4.41801776948587,0.375581263292163));
#13605=CARTESIAN_POINT('Ctrl Pts',(85.325724481569,-4.40709490668166,0.500877160188369));
#13606=CARTESIAN_POINT('Ctrl Pts',(85.3195294832927,-4.39078493141124,0.625852307579887));
#13607=CARTESIAN_POINT('Ctrl Pts',(85.3133461040938,-4.36916256993669,0.750018636766457));
#13608=CARTESIAN_POINT('Ctrl Pts',(85.307168464745,-4.34756027986803,0.874069705980425));
#13609=CARTESIAN_POINT('Ctrl Pts',(85.3010026794321,-4.32065571810597,0.997313514097945));
#13610=CARTESIAN_POINT('Ctrl Pts',(85.2949088018228,-4.28856072520909,1.11927693375167));
#13611=CARTESIAN_POINT('Ctrl Pts',(85.2908108730481,-4.26697791647055,1.2012932522454));
#13612=CARTESIAN_POINT('Ctrl Pts',(85.2869118605903,-4.24277054945837,1.28265283961973));
#13613=CARTESIAN_POINT('Ctrl Pts',(85.2830812618982,-4.21622777153665,1.36325866850456));
#13614=CARTESIAN_POINT('Ctrl Pts',(85.2812191292538,-4.20332478241829,1.40244281629966));
#13615=CARTESIAN_POINT('Ctrl Pts',(85.2793731636828,-4.18986972440365,1.44144960587744));
#13616=CARTESIAN_POINT('Ctrl Pts',(85.2775283734857,-4.17589453858595,1.48027215448857));
#13617=CARTESIAN_POINT('Ctrl Pts',(85.2697398901285,-4.11689297714989,1.64417630695318));
#13618=CARTESIAN_POINT('Ctrl Pts',(85.2619544711741,-4.04865181528642,1.80481341257982));
#13619=CARTESIAN_POINT('Ctrl Pts',(85.2541669226034,-3.97165771867034,1.96116259370312));
#13620=CARTESIAN_POINT('Ctrl Pts',(85.2506806541404,-3.9371896073732,2.0311557647776));
#13621=CARTESIAN_POINT('Ctrl Pts',(85.2471939527207,-3.90096660633359,2.10028946703939));
#13622=CARTESIAN_POINT('Ctrl Pts',(85.2437063512401,-3.86302935653635,2.16847054002379));
#13623=CARTESIAN_POINT('Ctrl Pts',(85.2393355443983,-3.81548482144543,2.25391788885295));
#13624=CARTESIAN_POINT('Ctrl Pts',(85.2349632968975,-3.7652452621893,2.33787320140798));
#13625=CARTESIAN_POINT('Ctrl Pts',(85.2307004097096,-3.71223605028654,2.42002879416054));
#13626=CARTESIAN_POINT('Ctrl Pts',(85.2294629596189,-3.69684829753027,2.44387728960959));
#13627=CARTESIAN_POINT('Ctrl Pts',(85.2282347247852,-3.6812273272569,2.46757384101803));
#13628=CARTESIAN_POINT('Ctrl Pts',(85.2270184154944,-3.6653717509357,2.49111022443572));
#13629=CARTESIAN_POINT('Ctrl Pts',(85.2226810167006,-3.60883024612882,2.57504173907688));
#13630=CARTESIAN_POINT('Ctrl Pts',(85.2185002056003,-3.54930026576319,2.65692809285175));
#13631=CARTESIAN_POINT('Ctrl Pts',(85.2143637396925,-3.48705788915787,2.73662776750612));
#13632=CARTESIAN_POINT('Ctrl Pts',(85.2133392630817,-3.47164234834229,2.75636694930846));
#13633=CARTESIAN_POINT('Ctrl Pts',(85.2123175066139,-3.45606029811023,2.7759722134224));
#13634=CARTESIAN_POINT('Ctrl Pts',(85.2112967650899,-3.44031566070746,2.79544182210765));
#13635=CARTESIAN_POINT('Ctrl Pts',(85.2061521108481,-3.36096088410859,2.8935708807936));
#13636=CARTESIAN_POINT('Ctrl Pts',(85.2010329451672,-3.27747677113758,2.98825187445984));
#13637=CARTESIAN_POINT('Ctrl Pts',(85.1958670671956,-3.19018387642686,3.07910075506622));
#13638=CARTESIAN_POINT('Ctrl Pts',(85.1906931541495,-3.10275520520107,3.17009094321484));
#13639=CARTESIAN_POINT('Ctrl Pts',(85.1854719470249,-3.01150566656215,3.25723667246366));
#13640=CARTESIAN_POINT('Ctrl Pts',(85.1801186357432,-2.91679888704007,3.34017703779908));
#13641=CARTESIAN_POINT('Ctrl Pts',(85.1752973944057,-2.83150509104349,3.41487389304535));
#13642=CARTESIAN_POINT('Ctrl Pts',(85.1703685282327,-2.74340758943231,3.48615979009815));
#13643=CARTESIAN_POINT('Ctrl Pts',(85.1652667799706,-2.65280287863538,3.55379345323013));
#13644=CARTESIAN_POINT('Ctrl Pts',(85.1652647448044,-2.6527667350155,3.55382043334396));
#13645=CARTESIAN_POINT('Ctrl Pts',(85.1652627096106,-2.65273059099647,3.5538474128773));
#13646=CARTESIAN_POINT('Ctrl Pts',(85.1652606743893,-2.65269444657834,3.55387439183014));
#13647=CARTESIAN_POINT('Ctrl Pts',(85.1600753925247,-2.56060667334183,3.62261063990077));
#13648=CARTESIAN_POINT('Ctrl Pts',(85.1547006967979,-2.46566074711065,3.6877668987319));
#13649=CARTESIAN_POINT('Ctrl Pts',(85.149213465117,-2.36818443293561,3.74913323468465));
#13650=CARTESIAN_POINT('Ctrl Pts',(85.1486566118364,-2.35829237652487,3.75536079121572));
#13651=CARTESIAN_POINT('Ctrl Pts',(85.1480985996017,-2.34837430506267,3.76154931927579));
#13652=CARTESIAN_POINT('Ctrl Pts',(85.1475395087587,-2.33843059095367,3.76769860148941));
#13653=CARTESIAN_POINT('Ctrl Pts',(85.141478539663,-2.23063318259331,3.83436148807664));
#13654=CARTESIAN_POINT('Ctrl Pts',(85.1352913460616,-2.11981621289668,3.8964122132986));
#13655=CARTESIAN_POINT('Ctrl Pts',(85.1290695032808,-2.00643204719541,3.9536190623625));
#13656=CARTESIAN_POINT('Ctrl Pts',(85.12285370252,-1.89315798864708,4.01077035796142));
#13657=CARTESIAN_POINT('Ctrl Pts',(85.116603670709,-1.77732185769731,4.06308752801176));
#13658=CARTESIAN_POINT('Ctrl Pts',(85.1103933370457,-1.65938377745455,4.11038104877906));
#13659=CARTESIAN_POINT('Ctrl Pts',(85.1056750483368,-1.56978055441894,4.14631220757636));
#13660=CARTESIAN_POINT('Ctrl Pts',(85.1009797936717,-1.47896125316684,4.17934463667908));
#13661=CARTESIAN_POINT('Ctrl Pts',(85.0964245021716,-1.38708885330889,4.20925442909443));
#13662=CARTESIAN_POINT('Ctrl Pts',(85.0949883328377,-1.35812378635327,4.21868423762538));
#13663=CARTESIAN_POINT('Ctrl Pts',(85.0935660756043,-1.3290544141682,4.22780354442039));
#13664=CARTESIAN_POINT('Ctrl Pts',(85.0921613947722,-1.29988688200897,4.23660505115098));
#13665=CARTESIAN_POINT('Ctrl Pts',(85.0872489806352,-1.19788292919405,4.2673854569922));
#13666=CARTESIAN_POINT('Ctrl Pts',(85.0824602450516,-1.09472882755048,4.29442923830735));
#13667=CARTESIAN_POINT('Ctrl Pts',(85.077692322407,-0.990756907868159,4.31787032279431));
#13668=CARTESIAN_POINT('Ctrl Pts',(85.0767746450963,-0.970745536303325,
4.32238200491949));
#13669=CARTESIAN_POINT('Ctrl Pts',(85.0758577387868,-0.950703716756279,
4.32676025572996));
#13670=CARTESIAN_POINT('Ctrl Pts',(85.0749408700586,-0.930633599828038,
4.33100606386856));
#13671=CARTESIAN_POINT('Ctrl Pts',(85.0673923349243,-0.765397314496613,
4.36596159340343));
#13672=CARTESIAN_POINT('Ctrl Pts',(85.0598462653068,-0.598241567400583,
4.39194463939876));
#13673=CARTESIAN_POINT('Ctrl Pts',(85.0522973114357,-0.4301706000107,4.40880275502221));
#13674=CARTESIAN_POINT('Ctrl Pts',(85.04848596313,-0.345314206962011,4.41731415296094));
#13675=CARTESIAN_POINT('Ctrl Pts',(85.044673895465,-0.260224722043043,4.42349865776892));
#13676=CARTESIAN_POINT('Ctrl Pts',(85.0408604921652,-0.175032810746617,
4.42733166758056));
#13677=CARTESIAN_POINT('Ctrl Pts',(85.0354698342498,-0.0546048321555523,
4.43275004142041));
#13678=CARTESIAN_POINT('Ctrl Pts',(85.0302412367628,0.0660442875316501,
4.43318368293072));
#13679=CARTESIAN_POINT('Ctrl Pts',(85.0252606189512,0.18643746193737,4.42840668878626));
#13680=CARTESIAN_POINT('Ctrl Pts',(85.0249886482198,0.19301163022839,4.42814583709275));
#13681=CARTESIAN_POINT('Ctrl Pts',(85.0247174169133,0.199585022546118,4.42786945021315));
#13682=CARTESIAN_POINT('Ctrl Pts',(85.0244469390212,0.206157556782235,4.42757749211126));
#13683=CARTESIAN_POINT('Ctrl Pts',(85.0192176276754,0.33322830397975,4.42193289098418));
#13684=CARTESIAN_POINT('Ctrl Pts',(85.0140479797323,0.459994220768434,4.41085131019553));
#13685=CARTESIAN_POINT('Ctrl Pts',(85.0088736397687,0.585954052039474,4.39436130789153));
#13686=CARTESIAN_POINT('Ctrl Pts',(85.0036961653171,0.711990186679063,4.3778613163496));
#13687=CARTESIAN_POINT('Ctrl Pts',(84.9985136303553,0.837219126886628,4.35594597195404));
#13688=CARTESIAN_POINT('Ctrl Pts',(84.9932455188829,0.961134268792317,4.32868874528195));
#13689=CARTESIAN_POINT('Ctrl Pts',(84.9883786009584,1.0756126408649,4.30350729539096));
#13690=CARTESIAN_POINT('Ctrl Pts',(84.9834381983927,1.18897018723484,4.27376641965414));
#13691=CARTESIAN_POINT('Ctrl Pts',(84.9783534039193,1.30080424095069,4.23956380318721));
#13692=CARTESIAN_POINT('Ctrl Pts',(84.9779263672656,1.31019640818819,4.23669136243107));
#13693=CARTESIAN_POINT('Ctrl Pts',(84.9774983121933,1.31957785908119,4.23378746134294));
#13694=CARTESIAN_POINT('Ctrl Pts',(84.9770691967007,1.32894837122947,4.23085216243986));
#13695=CARTESIAN_POINT('Ctrl Pts',(84.9746439662741,1.38190765973384,4.21426274459428));
#13696=CARTESIAN_POINT('Ctrl Pts',(84.9721847899234,1.43451645852858,4.19667080485617));
#13697=CARTESIAN_POINT('Ctrl Pts',(84.9696839599123,1.48673212258517,4.17809033243677));
#13698=CARTESIAN_POINT('Ctrl Pts',(84.9696819247138,1.48677461617353,4.17807521147717));
#13699=CARTESIAN_POINT('Ctrl Pts',(84.9696798894877,1.48681710950168,4.17806008986295));
#13700=CARTESIAN_POINT('Ctrl Pts',(84.9696778542341,1.48685960256962,4.17804496759413));
#13701=CARTESIAN_POINT('Ctrl Pts',(84.9644925752988,1.59512051017262,4.13951749412701));
#13702=CARTESIAN_POINT('Ctrl Pts',(84.9591178827597,1.70198674692963,4.0966265206881));
#13703=CARTESIAN_POINT('Ctrl Pts',(84.9536306546941,1.80710187557081,4.04952842474458));
#13704=CARTESIAN_POINT('Ctrl Pts',(84.9530738061195,1.81776904829537,4.0447488698801));
#13705=CARTESIAN_POINT('Ctrl Pts',(84.9525157986131,1.82841816474237,4.03992602651722));
#13706=CARTESIAN_POINT('Ctrl Pts',(84.9519567125193,1.83904883754031,4.03506008405304));
#13707=CARTESIAN_POINT('Ctrl Pts',(84.9458957520418,1.9542942145772,3.98230920133997));
#13708=CARTESIAN_POINT('Ctrl Pts',(84.9397085677023,2.06737541948516,3.92448822190028));
#13709=CARTESIAN_POINT('Ctrl Pts',(84.9334867347874,2.17784880585476,3.86184514143038));
#13710=CARTESIAN_POINT('Ctrl Pts',(84.9272709438731,2.28821491189869,3.79926289344054));
#13711=CARTESIAN_POINT('Ctrl Pts',(84.9210209225093,2.39597847332284,3.73186821447881));
#13712=CARTESIAN_POINT('Ctrl Pts',(84.9148105998528,2.50072665476181,3.65993894890574));
#13713=CARTESIAN_POINT('Ctrl Pts',(84.9100923213472,2.58030884723625,3.60529085307492));
#13714=CARTESIAN_POINT('Ctrl Pts',(84.9053970771899,2.65815290072415,3.54802354859147));
#13715=CARTESIAN_POINT('Ctrl Pts',(84.9008417967757,2.73398211261954,3.48814852671847));
#13716=CARTESIAN_POINT('Ctrl Pts',(84.8994056285702,2.75788920357092,3.46927140063666));
#13717=CARTESIAN_POINT('Ctrl Pts',(84.8979833725685,2.7815957190102,3.45013531491955));
#13718=CARTESIAN_POINT('Ctrl Pts',(84.896578693098,2.80509217788893,3.43074133727564));
#13719=CARTESIAN_POINT('Ctrl Pts',(84.891666288651,2.88726331480333,3.36291727916896));
#13720=CARTESIAN_POINT('Ctrl Pts',(84.8868775629567,2.96696244339537,3.2920643159296));
#13721=CARTESIAN_POINT('Ctrl Pts',(84.8821096502108,3.04411676486044,3.21853327559953));
#13722=CARTESIAN_POINT('Ctrl Pts',(84.8811919761277,3.05896655867597,3.2043808500813));
#13723=CARTESIAN_POINT('Ctrl Pts',(84.8802750730439,3.07372219006676,3.19012910601789));
#13724=CARTESIAN_POINT('Ctrl Pts',(84.8793582075413,3.08838328943348,3.17578038132092));
#13725=CARTESIAN_POINT('Ctrl Pts',(84.8718096813903,3.20908768027593,3.05764776175447));
#13726=CARTESIAN_POINT('Ctrl Pts',(84.8642636207654,3.32338920208233,2.93294302913735));
#13727=CARTESIAN_POINT('Ctrl Pts',(84.8567146758861,3.43060419465878,2.8024174136542));
#13728=CARTESIAN_POINT('Ctrl Pts',(84.8529033446259,3.48473518373024,2.73651729562523));
#13729=CARTESIAN_POINT('Ctrl Pts',(84.8490912940106,3.53705892944319,2.66913308306512));
#13730=CARTESIAN_POINT('Ctrl Pts',(84.8452779077678,3.5874825124696,2.60035987757172));
#13731=CARTESIAN_POINT('Ctrl Pts',(84.8398870676215,3.65876442791117,2.5031377936897));
#13732=CARTESIAN_POINT('Ctrl Pts',(84.834658308312,3.72602025675175,2.40296772540271));
#13733=CARTESIAN_POINT('Ctrl Pts',(84.8296775451296,3.78879745195251,2.30012150739739));
#13734=CARTESIAN_POINT('Ctrl Pts',(84.8294057559354,3.79222306418852,2.29450941750232));
#13735=CARTESIAN_POINT('Ctrl Pts',(84.829134705185,3.79563533511922,2.28888937065754));
#13736=CARTESIAN_POINT('Ctrl Pts',(84.8288644068382,3.79903418938342,2.28326141512133));
#13737=CARTESIAN_POINT('Ctrl Pts',(84.8236351120371,3.86478971895968,2.17438084303772));
#13738=CARTESIAN_POINT('Ctrl Pts',(84.8184654813944,3.92585147626731,2.06273948891568));
#13739=CARTESIAN_POINT('Ctrl Pts',(84.8132911594918,3.981965313625,1.94877034131851));
#13740=CARTESIAN_POINT('Ctrl Pts',(84.8081137030104,4.03811314446976,1.83473215177149));
#13741=CARTESIAN_POINT('Ctrl Pts',(84.8029311867842,4.08930667195149,1.71836324852354));
#13742=CARTESIAN_POINT('Ctrl Pts',(84.7976630947116,4.13532615997803,1.60012597256214));
#13743=CARTESIAN_POINT('Ctrl Pts',(84.7927961893516,4.17784107616579,1.49089294774299));
#13744=CARTESIAN_POINT('Ctrl Pts',(84.78785579976,4.21594011018023,1.38006477453644));
#13745=CARTESIAN_POINT('Ctrl Pts',(84.7827710182219,4.24948130381418,1.2680307221417));
#13746=CARTESIAN_POINT('Ctrl Pts',(84.7823439884463,4.25229815804497,1.25862188601248));
#13747=CARTESIAN_POINT('Ctrl Pts',(84.7819159402795,4.25508288962256,1.24920452565539));
#13748=CARTESIAN_POINT('Ctrl Pts',(84.7814868317212,4.25783542727072,1.23977886080998));
#13749=CARTESIAN_POINT('Ctrl Pts',(84.7790614671213,4.27339304606401,1.18650405796183));
#13750=CARTESIAN_POINT('Ctrl Pts',(84.7766021526623,4.28792190026075,1.1329650723735));
#13751=CARTESIAN_POINT('Ctrl Pts',(84.7741011792086,4.3014099859364,1.07920515793332));
#13752=CARTESIAN_POINT('Ctrl Pts',(84.7740991439519,4.30142096234921,1.07916140887747));
#13753=CARTESIAN_POINT('Ctrl Pts',(84.7740971086676,4.30143193807291,1.07911765967523));
#13754=CARTESIAN_POINT('Ctrl Pts',(84.7740950733557,4.30144291310753,1.07907391032659));
#13755=CARTESIAN_POINT('Ctrl Pts',(84.768909803381,4.32940350105146,0.967615718873223));
#13756=CARTESIAN_POINT('Ctrl Pts',(84.763535117755,4.35295944008393,0.854898914033085));
#13757=CARTESIAN_POINT('Ctrl Pts',(84.7580478939663,4.37204324863032,0.741306830386417));
#13758=CARTESIAN_POINT('Ctrl Pts',(84.7574910265083,4.37397995694803,0.729779009160925));
#13759=CARTESIAN_POINT('Ctrl Pts',(84.7569330000111,4.37587062545103,0.718242213346182));
#13760=CARTESIAN_POINT('Ctrl Pts',(84.7563738948267,4.37771519698071,0.706696870372616));
#13761=CARTESIAN_POINT('Ctrl Pts',(84.7503129183795,4.39771126374356,0.581539648120451));
#13762=CARTESIAN_POINT('Ctrl Pts',(84.7441257143383,4.4122879629984,0.455372437180053));
#13763=CARTESIAN_POINT('Ctrl Pts',(84.7379038586095,4.42140570754389,0.328701950375454));
#13764=CARTESIAN_POINT('Ctrl Pts',(84.7316880450157,4.43051459771433,0.202154475132937));
#13765=CARTESIAN_POINT('Ctrl Pts',(84.7254379978752,4.43417550512059,0.075104696430171));
#13766=CARTESIAN_POINT('Ctrl Pts',(84.7192276472584,4.43239076643115,-0.0519497654959621));
#13767=CARTESIAN_POINT('Ctrl Pts',(84.7145096587603,4.43103490472084,-0.148472736096043));
#13768=CARTESIAN_POINT('Ctrl Pts',(84.7098147003148,4.4265359915693,-0.245001378756047));
#13769=CARTESIAN_POINT('Ctrl Pts',(84.7052597085182,4.41875015260918,-0.341299084631016));
#13770=CARTESIAN_POINT('Ctrl Pts',(84.7038232361851,4.41629479313635,-0.371667743107352));
#13771=CARTESIAN_POINT('Ctrl Pts',(84.7024006840014,4.41351257292165,-0.402013046553423));
#13772=CARTESIAN_POINT('Ctrl Pts',(84.700995719546,4.4103991195604,-0.432326506843429));
#13773=CARTESIAN_POINT('Ctrl Pts',(84.6960830564247,4.39951247581047,-0.538321941723752));
#13774=CARTESIAN_POINT('Ctrl Pts',(84.6912940568784,4.38473411194135,-0.643939410514095));
#13775=CARTESIAN_POINT('Ctrl Pts',(84.6865258619715,4.3663156351685,-0.748923772186185));
#13776=CARTESIAN_POINT('Ctrl Pts',(84.6856084689167,4.36277194976964,-0.769122595039711));
#13777=CARTESIAN_POINT('Ctrl Pts',(84.6846918459903,4.35909348503392,-0.789298133509308));
#13778=CARTESIAN_POINT('Ctrl Pts',(84.6837752606268,4.35528197981159,-0.80944878521036));
#13779=CARTESIAN_POINT('Ctrl Pts',(84.6762267057085,4.32389226136465,-0.975399832506024));
#13780=CARTESIAN_POINT('Ctrl Pts',(84.6686806166527,4.28348300576916,-1.13966608036638));
#13781=CARTESIAN_POINT('Ctrl Pts',(84.6611316436492,4.23430036531949,-1.30126205165788));
#13782=CARTESIAN_POINT('Ctrl Pts',(84.6573203316184,4.20946912149827,-1.38284833752986));
#13783=CARTESIAN_POINT('Ctrl Pts',(84.6535083003208,4.18240079675737,-1.46375343855993));
#13784=CARTESIAN_POINT('Ctrl Pts',(84.6496949334886,4.15312301906299,-1.54384729969441));
#13785=CARTESIAN_POINT('Ctrl Pts',(84.6443132190019,4.11180398334093,-1.65688187301069));
#13786=CARTESIAN_POINT('Ctrl Pts',(84.639092697203,4.06581574754515,-1.76820634527985));
#13787=CARTESIAN_POINT('Ctrl Pts',(84.6341194783051,4.01513272168606,-1.87729568176754));
#13788=CARTESIAN_POINT('Ctrl Pts',(84.6338392039288,4.0122763918614,-1.88344360052497));
#13789=CARTESIAN_POINT('Ctrl Pts',(84.6335597150067,4.00940515807036,-1.88958440849035));
#13790=CARTESIAN_POINT('Ctrl Pts',(84.6332810269519,4.00651901836426,-1.8957180075007));
#13791=CARTESIAN_POINT('Ctrl Pts',(84.6280517137449,3.95236338369587,-2.01080909145097));
#13792=CARTESIAN_POINT('Ctrl Pts',(84.6228820688287,3.89330774160362,-2.12352459141227));
#13793=CARTESIAN_POINT('Ctrl Pts',(84.6177077380327,3.8295715259579,-2.23341293355516));
#13794=CARTESIAN_POINT('Ctrl Pts',(84.6125302727593,3.76579670054097,-2.34336784324847));
#13795=CARTESIAN_POINT('Ctrl Pts',(84.6073477531349,3.6973353322639,-2.45049190190229));
#13796=CARTESIAN_POINT('Ctrl Pts',(84.6020796641393,3.62445036165115,-2.55434589972039));
#13797=CARTESIAN_POINT('Ctrl Pts',(84.5972127429459,3.55711562063874,-2.65029135990778));
#13798=CARTESIAN_POINT('Ctrl Pts',(84.5922723424912,3.48600498536139,-2.74344620822685));
#13799=CARTESIAN_POINT('Ctrl Pts',(84.5871875548635,3.41136371001468,-2.83347647361782));
#13800=CARTESIAN_POINT('Ctrl Pts',(84.5867605459365,3.40509550508114,-2.8410370110158));
#13801=CARTESIAN_POINT('Ctrl Pts',(84.5863325187537,3.39880239828021,-2.84857554335884));
#13802=CARTESIAN_POINT('Ctrl Pts',(84.5859034313212,3.39248453294577,-2.85609188952173));
#13803=CARTESIAN_POINT('Ctrl Pts',(84.5834781257411,3.35677443544996,-2.89857608949763));
#13804=CARTESIAN_POINT('Ctrl Pts',(84.5810188731415,3.32027412338363,-2.94035063029836));
#13805=CARTESIAN_POINT('Ctrl Pts',(84.5785179649191,3.28301293624369,-2.98138154243981));
#13806=CARTESIAN_POINT('Ctrl Pts',(84.5785159299288,3.28298261679641,-2.98141492931428));
#13807=CARTESIAN_POINT('Ctrl Pts',(84.5785138949109,3.28295229684535,-2.98144831569655));
#13808=CARTESIAN_POINT('Ctrl Pts',(84.5785118598654,3.28292197639053,-2.98148170158665));
#13809=CARTESIAN_POINT('Ctrl Pts',(84.5733265574052,3.20566535957455,-3.06654905737755));
#13810=CARTESIAN_POINT('Ctrl Pts',(84.5679518428513,3.12491911275222,-3.14864850413186));
#13811=CARTESIAN_POINT('Ctrl Pts',(84.5624645943197,3.04096485078219,-3.22751134131508));
#13812=CARTESIAN_POINT('Ctrl Pts',(84.5619077499984,3.03244519766962,-3.23551431818019));
#13813=CARTESIAN_POINT('Ctrl Pts',(84.5613497467876,3.02389255180424,-3.24348395767438));
#13814=CARTESIAN_POINT('Ctrl Pts',(84.560790665029,3.01530723717742,-3.25141997527823));
#13815=CARTESIAN_POINT('Ctrl Pts',(84.5547296888236,2.92223428878533,-3.33745392848651));
#13816=CARTESIAN_POINT('Ctrl Pts',(84.5485424907892,2.82531604959927,-3.41953766354237));
#13817=CARTESIAN_POINT('Ctrl Pts',(84.5423206455941,2.72495227604094,-3.49735729128607));
#13818=CARTESIAN_POINT('Ctrl Pts',(84.5361048423106,2.6246859637701,-3.5751013499191));
#13819=CARTESIAN_POINT('Ctrl Pts',(84.529854809988,2.52098100948511,-3.64858989306717));
#13820=CARTESIAN_POINT('Ctrl Pts',(84.5236444767993,2.41425284641874,-3.717548962688));
#13821=CARTESIAN_POINT('Ctrl Pts',(84.5189257891911,2.33315947425737,-3.7699449126978));
#13822=CARTESIAN_POINT('Ctrl Pts',(84.5142301400925,2.25031820586455,-3.81972745306807));
#13823=CARTESIAN_POINT('Ctrl Pts',(84.5096744486561,2.16584629455141,-3.86664565444101));
#13824=CARTESIAN_POINT('Ctrl Pts',(84.5082386601763,2.13922381609311,-3.88143256746258));
#13825=CARTESIAN_POINT('Ctrl Pts',(84.5068167734316,2.11243971047828,-3.8959347854256));
#13826=CARTESIAN_POINT('Ctrl Pts',(84.505412448532,2.08549861207607,-3.91014397891237));
#13827=CARTESIAN_POINT('Ctrl Pts',(84.500500330476,1.99126268708196,-3.95984560843227));
#13828=CARTESIAN_POINT('Ctrl Pts',(84.4957119095192,1.89518400202996,-4.0060996746415));
#13829=CARTESIAN_POINT('Ctrl Pts',(84.4909443119702,1.79761431116414,-4.04897415816643));
#13830=CARTESIAN_POINT('Ctrl Pts',(84.4900262694309,1.77882641519906,-4.05723001435369));
#13831=CARTESIAN_POINT('Ctrl Pts',(84.489108999,1.75998309001578,-4.06536061625154));
#13832=CARTESIAN_POINT('Ctrl Pts',(84.4881917661738,1.74108663839054,-4.07336652430806));
#13833=CARTESIAN_POINT('Ctrl Pts',(84.4806432389444,1.5855749999614,-4.13925253844839));
#13834=CARTESIAN_POINT('Ctrl Pts',(84.4730971767776,1.42646473439164,-4.19669820861065));
#13835=CARTESIAN_POINT('Ctrl Pts',(84.4655482299722,1.26471243690291,-4.24536198986576));
#13836=CARTESIAN_POINT('Ctrl Pts',(84.4617368033983,1.18304448759641,-4.26993209664203));
#13837=CARTESIAN_POINT('Ctrl Pts',(84.4579246573404,1.10070306845423,-4.29226263505166));
#13838=CARTESIAN_POINT('Ctrl Pts',(84.4541111755068,1.01781174310843,-4.31230448362946));
#13839=CARTESIAN_POINT('Ctrl Pts',(84.4484261205266,0.894239175431847,-4.3421824314052));
#13840=CARTESIAN_POINT('Ctrl Pts',(84.4429217562405,0.76936510175984,-4.36666473639337));
#13841=CARTESIAN_POINT('Ctrl Pts',(84.4376979694913,0.643690135002427,-4.38538581583833));
#13842=CARTESIAN_POINT('Ctrl Pts',(84.4324686290142,0.517881555483126,-4.40412679881058));
#13843=CARTESIAN_POINT('Ctrl Pts',(84.4272989443257,0.391333239082584,-4.41747267370568));
#13844=CARTESIAN_POINT('Ctrl Pts',(84.4221245584116,0.264542667669082,-4.42535568566965));
#13845=CARTESIAN_POINT('Ctrl Pts',(84.4169470381692,0.13767529424048,-4.43324347268272));
#13846=CARTESIAN_POINT('Ctrl Pts',(84.4117644481786,0.0105654297978427,
-4.43566138153736));
#13847=CARTESIAN_POINT('Ctrl Pts',(84.4064962713937,-0.116275610554298,
-4.4325847207063));
#13848=CARTESIAN_POINT('Ctrl Pts',(84.4016293336883,-0.233456082488926,
-4.4297423869698));
#13849=CARTESIAN_POINT('Ctrl Pts',(84.3966889037664,-0.350407633567806,
-4.42221048502865));
#13850=CARTESIAN_POINT('Ctrl Pts',(84.3916040760287,-0.466716354271229,
-4.41000795340358));
#13851=CARTESIAN_POINT('Ctrl Pts',(84.391176991259,-0.476485354472302,-4.40898303856334));
#13852=CARTESIAN_POINT('Ctrl Pts',(84.3907488878128,-0.486249846560294,
-4.40792518846741));
#13853=CARTESIAN_POINT('Ctrl Pts',(84.390319723676,-0.496009600215878,-4.40683442198824));
#13854=CARTESIAN_POINT('Ctrl Pts',(84.387894843512,-0.551154545982175,-4.40067133012542));
#13855=CARTESIAN_POINT('Ctrl Pts',(84.3854360262954,-0.606147076768305,
-4.39345753784936));
#13856=CARTESIAN_POINT('Ctrl Pts',(84.3829355680468,-0.66094268088986,-4.38519862474495));
#13857=CARTESIAN_POINT('Ctrl Pts',(84.382933532696,-0.660987284023301,-4.38519190206328));
#13858=CARTESIAN_POINT('Ctrl Pts',(84.3829314973177,-0.6610318870264,-4.38518517868924));
#13859=CARTESIAN_POINT('Ctrl Pts',(84.3829294619118,-0.661076489899159,
-4.38517845462283));
#13860=CARTESIAN_POINT('Ctrl Pts',(84.3777441956494,-0.774703835395292,
-4.36804866522549));
#13861=CARTESIAN_POINT('Ctrl Pts',(84.3723695177718,-0.88779606058497,-4.34636933738174));
#13862=CARTESIAN_POINT('Ctrl Pts',(84.3668823074273,-0.999973416805149,
-4.32022585152307));
#13863=CARTESIAN_POINT('Ctrl Pts',(84.3663254894094,-1.01135668247584,-4.31757292534336));
#13864=CARTESIAN_POINT('Ctrl Pts',(84.365767512611,-1.02273049790092,-4.31487406332162));
#13865=CARTESIAN_POINT('Ctrl Pts',(84.365208457365,-1.03409444672231,-4.31212937732032));
#13866=CARTESIAN_POINT('Ctrl Pts',(84.3591475471469,-1.1572949247151,-4.28237329229963));
#13867=CARTESIAN_POINT('Ctrl Pts',(84.3529604176001,-1.2793400076234,-4.24722710726337));
#13868=CARTESIAN_POINT('Ctrl Pts',(84.346738643613,-1.39974684446633,-4.20684946448488));
#13869=CARTESIAN_POINT('Ctrl Pts',(84.3405229114828,-1.52003675631752,-4.16651103173526));
#13870=CARTESIAN_POINT('Ctrl Pts',(84.3342729530153,-1.63869175079973,-4.12095164052296));
#13871=CARTESIAN_POINT('Ctrl Pts',(84.3280626968707,-1.75525351555293,-4.07036511954236));
#13872=CARTESIAN_POINT('Ctrl Pts',(84.323344383073,-1.84381266192753,-4.03193142625033));
#13873=CARTESIAN_POINT('Ctrl Pts',(84.3186491065442,-1.93116619998183,-3.99059460369246));
#13874=CARTESIAN_POINT('Ctrl Pts',(84.3140937959104,-2.01704032526029,-3.94631306123798));
#13875=CARTESIAN_POINT('Ctrl Pts',(84.3126577269723,-2.04411228012874,-3.93235323439904));
#13876=CARTESIAN_POINT('Ctrl Pts',(84.3112355683443,-2.07103686167745,-3.91810093225873));
#13877=CARTESIAN_POINT('Ctrl Pts',(84.3098309834969,-2.09780456156354,-3.90355539143292));
#13878=CARTESIAN_POINT('Ctrl Pts',(84.3049187094006,-2.19141961017728,-3.8526850694659));
#13879=CARTESIAN_POINT('Ctrl Pts',(84.3001301197621,-2.28318710933881,-3.7983694526866));
#13880=CARTESIAN_POINT('Ctrl Pts',(84.2953623456716,-2.37296857833148,-3.74093898603706));
#13881=CARTESIAN_POINT('Ctrl Pts',(84.2944446023704,-2.39025050909643,-3.72988426216618));
#13882=CARTESIAN_POINT('Ctrl Pts',(84.293527630326,-2.40745898081416,-3.7187140383902));
#13883=CARTESIAN_POINT('Ctrl Pts',(84.2926106958682,-2.4245931838124,-3.70743053955982));
#13884=CARTESIAN_POINT('Ctrl Pts',(84.2850622258382,-2.56564690550592,-3.61454150912677));
#13885=CARTESIAN_POINT('Ctrl Pts',(84.2775162212794,-2.70167171791562,-3.51397803803153));
#13886=CARTESIAN_POINT('Ctrl Pts',(84.2699673323685,-2.83185301388745,-3.4063468653672));
#13887=CARTESIAN_POINT('Ctrl Pts',(84.2661560849157,-2.89757833300751,-3.35200654621597));
#13888=CARTESIAN_POINT('Ctrl Pts',(84.2623441181025,-2.96181337970296,-3.29586420792149));
#13889=CARTESIAN_POINT('Ctrl Pts',(84.2585308156723,-3.02444877978825,-3.23799543932097));
#13890=CARTESIAN_POINT('Ctrl Pts',(84.2531361978723,-3.11305807590203,-3.15612942033363));
#13891=CARTESIAN_POINT('Ctrl Pts',(84.2479040427514,-3.19827388489918,-3.07059505341164));
#13892=CARTESIAN_POINT('Ctrl Pts',(84.2429201846493,-3.27959931121367,-2.98157340683114));
#13893=CARTESIAN_POINT('Ctrl Pts',(84.2426519708598,-3.28397596085487,-2.97678257356753));
#13894=CARTESIAN_POINT('Ctrl Pts',(84.2423844761919,-3.28834133566107,-2.97198165050621));
#13895=CARTESIAN_POINT('Ctrl Pts',(84.2421177140242,-3.29269535571472,-2.96717066938321));
#13896=CARTESIAN_POINT('Ctrl Pts',(84.236888511953,-3.37804497961775,-2.87286347180652));
#13897=CARTESIAN_POINT('Ctrl Pts',(84.2317189767506,-3.45931499008182,-2.7749495005523));
#13898=CARTESIAN_POINT('Ctrl Pts',(84.2265447526407,-3.5361731913615,-2.67380519287902));
#13899=CARTESIAN_POINT('Ctrl Pts',(84.2213673934426,-3.61307796140822,-2.57259960136585));
#13900=CARTESIAN_POINT('Ctrl Pts',(84.2161849768733,-3.68556521370341,-2.4681595865901));
#13901=CARTESIAN_POINT('Ctrl Pts',(84.2109169859668,-3.75333092100466,-2.36089697216956));
#13902=CARTESIAN_POINT('Ctrl Pts',(84.2060501515979,-3.81593628217304,-2.26180238608621));
#13903=CARTESIAN_POINT('Ctrl Pts',(84.2011098336268,-3.8745120190635,-2.16029823643245));
#13904=CARTESIAN_POINT('Ctrl Pts',(84.1960251220409,-3.92884440752957,-2.05673948987575));
#13905=CARTESIAN_POINT('Ctrl Pts',(84.1955981220718,-3.93340709074217,-2.0480429137124));
#13906=CARTESIAN_POINT('Ctrl Pts',(84.1951701038138,-3.93793987598769,-2.03933183384053));
#13907=CARTESIAN_POINT('Ctrl Pts',(84.1947410252724,-3.94244265133404,-2.03060645229457));
#13908=CARTESIAN_POINT('Ctrl Pts',(84.1923149363545,-3.96790217054373,-1.98127154171295));
#13909=CARTESIAN_POINT('Ctrl Pts',(84.1898548759893,-3.99240178177722,-1.9314804486622));
#13910=CARTESIAN_POINT('Ctrl Pts',(84.1873531275102,-4.01592141876326,-1.88127337373804));
#13911=CARTESIAN_POINT('Ctrl Pts',(84.1873510918653,-4.01594055643057,-1.88123252079897));
#13912=CARTESIAN_POINT('Ctrl Pts',(84.1873490561927,-4.01595969344922,-1.88119166758441));
#13913=CARTESIAN_POINT('Ctrl Pts',(84.1873470204926,-4.01597882981921,-1.88115081409439));
#13914=CARTESIAN_POINT('Ctrl Pts',(84.1819697230983,-4.06652750835006,-1.7732364115609));
#13915=CARTESIAN_POINT('Ctrl Pts',(84.1763910602686,-4.11265933192718,-1.66314804805023));
#13916=CARTESIAN_POINT('Ctrl Pts',(84.1706955902453,-4.15424332898281,-1.5512634750962));
#13917=CARTESIAN_POINT('Ctrl Pts',(84.1698688634138,-4.16027946050242,-1.53502285261677));
#13918=CARTESIAN_POINT('Ctrl Pts',(84.1690396754526,-4.16621977557407,-1.51874447338153));
#13919=CARTESIAN_POINT('Ctrl Pts',(84.1682082849763,-4.1720638824027,-1.50242958347748));
#13920=CARTESIAN_POINT('Ctrl Pts',(84.1621129362214,-4.21491001824171,-1.38281678215043));
#13921=CARTESIAN_POINT('Ctrl Pts',(84.1558997937435,-4.25258494005077,-1.26123583913524));
#13922=CARTESIAN_POINT('Ctrl Pts',(84.1496578445298,-4.28497060102772,-1.13814119430532));
#13923=CARTESIAN_POINT('Ctrl Pts',(84.1492041116699,-4.2873247436316,-1.12919333469826));
#13924=CARTESIAN_POINT('Ctrl Pts',(84.1487502265962,-4.28965093504631,-1.1202374993918));
#13925=CARTESIAN_POINT('Ctrl Pts',(84.1482962234882,-4.2919491288373,-1.11127387361339));
#13926=CARTESIAN_POINT('Ctrl Pts',(84.1416095743663,-4.32579738939976,-0.979255789620047));
#13927=CARTESIAN_POINT('Ctrl Pts',(84.134897742431,-4.35357361761577,-0.845541944315518));
#13928=CARTESIAN_POINT('Ctrl Pts',(84.1282458234568,-4.37517089418641,-0.710689438469849));
#13929=CARTESIAN_POINT('Ctrl Pts',(84.1237021614488,-4.38992313717226,-0.618577040548796));
#13930=CARTESIAN_POINT('Ctrl Pts',(84.1191966943683,-4.40177509059477,-0.525927551545028));
#13931=CARTESIAN_POINT('Ctrl Pts',(84.1148472705922,-4.41053065276273,-0.432914202617163));
#13932=CARTESIAN_POINT('Ctrl Pts',(84.1128481987243,-4.41455486353612,-0.390163627195017));
#13933=CARTESIAN_POINT('Ctrl Pts',(84.1108820907501,-4.41792484474684,-0.347336899647861));
#13934=CARTESIAN_POINT('Ctrl Pts',(84.1089603889782,-4.42062115446675,-0.304454516660194));
#13935=CARTESIAN_POINT('Ctrl Pts',(84.1044418844722,-4.42696099751471,-0.20362501044392));
#13936=CARTESIAN_POINT('Ctrl Pts',(84.0999225009031,-4.43000245478287,-0.102516986223067));
#13937=CARTESIAN_POINT('Ctrl Pts',(84.0954003870484,-4.42975191188515,-0.00133220471272644));
#13938=CARTESIAN_POINT('Ctrl Pts',(84.0953986853364,-4.42975181744819,-0.00129412797191142));
#13939=CARTESIAN_POINT('Ctrl Pts',(84.0921041236228,-4.42956868394745,0.0724235029283445));
#13940=CARTESIAN_POINT('Ctrl Pts',(84.0888129452018,-4.4276388654098,0.146073633444381));
#13941=CARTESIAN_POINT('Ctrl Pts',(84.0855227855576,-4.42397300444274,0.219615246120854));
#13942=CARTESIAN_POINT('Ctrl Pts',(84.0832767518464,-4.42147049751198,0.26981856727126));
#13943=CARTESIAN_POINT('Ctrl Pts',(84.081031192899,-4.41815876163643,0.319971342296661));
#13944=CARTESIAN_POINT('Ctrl Pts',(84.0787853565039,-4.41403849979053,0.370060518426921));
#13945=CARTESIAN_POINT('Ctrl Pts',(84.0766447228571,-4.41011124526732,0.417803344217714));
#13946=CARTESIAN_POINT('Ctrl Pts',(84.0745040431029,-4.40544960649604,0.465483779962639));
#13947=CARTESIAN_POINT('Ctrl Pts',(84.0723635194703,-4.40005552138737,0.513071474916498));
#13948=CARTESIAN_POINT('Ctrl Pts',(84.0683690128851,-4.38998942907243,0.601876549513941));
#13949=CARTESIAN_POINT('Ctrl Pts',(84.0643746841183,-4.37737225064415,0.690366878393935));
#13950=CARTESIAN_POINT('Ctrl Pts',(84.0603796133334,-4.36220899928437,0.778394604056078));
#13951=CARTESIAN_POINT('Ctrl Pts',(84.05617274016,-4.34624185406891,0.871089201361364));
#13952=CARTESIAN_POINT('Ctrl Pts',(84.0521774134784,-4.32708977131361,0.963202639840204));
#13953=CARTESIAN_POINT('Ctrl Pts',(84.0482733884729,-4.30496998710146,1.05454490782526));
#13954=CARTESIAN_POINT('Ctrl Pts',(84.0465086388677,-4.29497110635664,1.09583466163947));
#13955=CARTESIAN_POINT('Ctrl Pts',(84.044762545315,-4.2843657224338,1.13696754074424));
#13956=CARTESIAN_POINT('Ctrl Pts',(84.0430240012982,-4.27317320049019,1.17792941784365));
#13957=CARTESIAN_POINT('Ctrl Pts',(84.0376734094523,-4.23872678091809,1.30399484010832));
#13958=CARTESIAN_POINT('Ctrl Pts',(84.032373050424,-4.19875456442782,1.42844930968254));
#13959=CARTESIAN_POINT('Ctrl Pts',(84.0270479533909,-4.15340577613371,1.55078471097965));
#13960=CARTESIAN_POINT('Ctrl Pts',(84.0217176986437,-4.10801306449197,1.67323860233045));
#13961=CARTESIAN_POINT('Ctrl Pts',(84.0163622131321,-4.05723291931334,1.79356913068581));
#13962=CARTESIAN_POINT('Ctrl Pts',(84.0108900377808,-4.0012607786246,1.91127096742671));
#13963=CARTESIAN_POINT('Ctrl Pts',(84.0060032934323,-3.95127671842411,2.01638068131246));
#13964=CARTESIAN_POINT('Ctrl Pts',(84.0010229837432,-3.89715180930192,2.11939486055675));
#13965=CARTESIAN_POINT('Ctrl Pts',(83.9958781590854,-3.83906274531618,2.219956617997));
#13966=CARTESIAN_POINT('Ctrl Pts',(83.9952521771515,-3.83199492337375,2.23219218433321));
#13967=CARTESIAN_POINT('Ctrl Pts',(83.9946237597193,-3.82486842011884,2.24439150798265));
#13968=CARTESIAN_POINT('Ctrl Pts',(83.9939927789906,-3.81768355643046,2.25655399880712));
#13969=CARTESIAN_POINT('Ctrl Pts',(83.9932545591512,-3.80927758034196,2.27078358081195));
#13970=CARTESIAN_POINT('Ctrl Pts',(83.9925128278645,-3.80079179029708,2.28496265396045));
#13971=CARTESIAN_POINT('Ctrl Pts',(83.9917673800263,-3.79222676466892,2.29909021385551));
#13972=CARTESIAN_POINT('Ctrl Pts',(83.9917653465489,-3.79220340047755,2.29912875186197));
#13973=CARTESIAN_POINT('Ctrl Pts',(83.9917633130438,-3.79218003569659,2.2991672894851));
#13974=CARTESIAN_POINT('Ctrl Pts',(83.9917612795111,-3.79215667032603,2.29920582672493));
#13975=CARTESIAN_POINT('Ctrl Pts',(83.9865757948938,-3.73257524862255,2.39747533769407));
#13976=CARTESIAN_POINT('Ctrl Pts',(83.9812009167659,-3.66900089073088,2.49349808630057));
#13977=CARTESIAN_POINT('Ctrl Pts',(83.9757135262295,-3.60165872173485,2.58695647398915));
#13978=CARTESIAN_POINT('Ctrl Pts',(83.9751567956568,-3.59482643158448,2.59643842016334));
#13979=CARTESIAN_POINT('Ctrl Pts',(83.97459890695,-3.58795539964775,2.6058939557739));
#13980=CARTESIAN_POINT('Ctrl Pts',(83.9740399403985,-3.58104588944113,2.61532273982873));
#13981=CARTESIAN_POINT('Ctrl Pts',(83.9679789452048,-3.50612457610737,2.71756108428501));
#13982=CARTESIAN_POINT('Ctrl Pts',(83.9617917577651,-3.4266736543611,2.81665643569426));
#13983=CARTESIAN_POINT('Ctrl Pts',(83.9555699461621,-3.34302557056066,2.91222427944364));
#13984=CARTESIAN_POINT('Ctrl Pts',(83.94935417531,-3.25945870060518,3.00769933646447));
#13985=CARTESIAN_POINT('Ctrl Pts',(83.9431041983205,-3.17170307474004,3.09965400179128));
#13986=CARTESIAN_POINT('Ctrl Pts',(83.9368939332264,-3.08011415524685,3.18773995994843));
#13987=CARTESIAN_POINT('Ctrl Pts',(83.9321714407092,-3.01046688892119,3.25472345774784));
#13988=CARTESIAN_POINT('Ctrl Pts',(83.9274720317323,-2.93860077278703,3.31947182220502));
#13989=CARTESIAN_POINT('Ctrl Pts',(83.9229125305786,-2.86458353598871,3.38171618169541));
#13990=CARTESIAN_POINT('Ctrl Pts',(83.921480437798,-2.84133547728902,3.40126649978011));
#13991=CARTESIAN_POINT('Ctrl Pts',(83.9200621472598,-2.81787550339761,3.42056954585345));
#13992=CARTESIAN_POINT('Ctrl Pts',(83.9186612788476,-2.79420655895491,3.43961634624809));
#13993=CARTESIAN_POINT('Ctrl Pts',(83.9137520717548,-2.71126104535474,3.50636400561238));
#13994=CARTESIAN_POINT('Ctrl Pts',(83.9089667419841,-2.62585089380582,3.57008342169783));
#13995=CARTESIAN_POINT('Ctrl Pts',(83.9042023368082,-2.53833398823929,3.63077443813605));
#13996=CARTESIAN_POINT('Ctrl Pts',(83.903280789688,-2.52140617683094,3.64251349670761));
#13997=CARTESIAN_POINT('Ctrl Pts',(83.902360025411,-2.50439941431259,3.65413933914884));
#13998=CARTESIAN_POINT('Ctrl Pts',(83.9014392989632,-2.48731609731623,3.6656520795929));
#13999=CARTESIAN_POINT('Ctrl Pts',(83.893890900357,-2.34726181028116,3.76003706671547));
#14000=CARTESIAN_POINT('Ctrl Pts',(83.8863449624767,-2.20206255364273,3.84682508637063));
#14001=CARTESIAN_POINT('Ctrl Pts',(83.8787961362334,-2.05259191981534,3.92549805073244));
#14002=CARTESIAN_POINT('Ctrl Pts',(83.8749840512519,-1.97711068074216,3.96522714453188));
#14003=CARTESIAN_POINT('Ctrl Pts',(83.8711712456039,-1.90054003840731,4.00288588696796));
#14004=CARTESIAN_POINT('Ctrl Pts',(83.8673571028617,-1.82299194579675,4.0384024029594));
#14005=CARTESIAN_POINT('Ctrl Pts',(83.861671776735,-1.70739947147196,4.09134299536656));
#14006=CARTESIAN_POINT('Ctrl Pts',(83.8561715279256,-1.58949550822084,4.13922841460962));
#14007=CARTESIAN_POINT('Ctrl Pts',(83.8509475525488,-1.46970726301584,4.18161804952431));
#14008=CARTESIAN_POINT('Ctrl Pts',(83.8457180259812,-1.34979172635732,4.2240527292448));
#14009=CARTESIAN_POINT('Ctrl Pts',(83.8405480859766,-1.2281190573001,4.26133255678184));
#14010=CARTESIAN_POINT('Ctrl Pts',(83.835373360171,-1.10516466997342,4.29329593792215));
#14011=CARTESIAN_POINT('Ctrl Pts',(83.830195501057,-0.982135833481593,4.32527867296346));
#14012=CARTESIAN_POINT('Ctrl Pts',(83.8250124873297,-0.857823707063181,
4.35193812240549));
#14013=CARTESIAN_POINT('Ctrl Pts',(83.8197437912569,-0.732725519128845,
4.37315232248143));
#14014=CARTESIAN_POINT('Ctrl Pts',(83.8148767348689,-0.617163731868134,
4.3927493359679));
#14015=CARTESIAN_POINT('Ctrl Pts',(83.809936115427,-0.500930638268043,4.40769966463376));
#14016=CARTESIAN_POINT('Ctrl Pts',(83.8048510408623,-0.384436097958309,
4.41794280566729));
#14017=CARTESIAN_POINT('Ctrl Pts',(83.8044235307491,-0.374642221096632,
4.41880396243646));
#14018=CARTESIAN_POINT('Ctrl Pts',(83.8039949996233,-0.36484647269912,4.41963186800146));
#14019=CARTESIAN_POINT('Ctrl Pts',(83.8035654053595,-0.355049083076931,
4.42042649680689));
#14020=CARTESIAN_POINT('Ctrl Pts',(83.8011431360686,-0.299806455297337,
4.42490701508921));
#14021=CARTESIAN_POINT('Ctrl Pts',(83.7986869927428,-0.244512795542103,
4.42832951566351));
#14022=CARTESIAN_POINT('Ctrl Pts',(83.7961892995956,-0.189212704827418,
4.43069097878495));
#14023=CARTESIAN_POINT('Ctrl Pts',(83.7961872624375,-0.189167601199163,
4.43069290483161));
#14024=CARTESIAN_POINT('Ctrl Pts',(83.7961852252519,-0.189122497566507,
4.43069483017255));
#14025=CARTESIAN_POINT('Ctrl Pts',(83.7961831880386,-0.189077393929466,
4.43069675480781));
#14026=CARTESIAN_POINT('Ctrl Pts',(83.7909980958776,-0.074280129178877,
4.43559531459573));
#14027=CARTESIAN_POINT('Ctrl Pts',(83.785623599497,0.0408613960656662,4.43592667179727));
#14028=CARTESIAN_POINT('Ctrl Pts',(83.7801365849949,0.155958163511104,4.43170203503521));
#14029=CARTESIAN_POINT('Ctrl Pts',(83.7795799531664,0.167634189533694,4.43127346549442));
#14030=CARTESIAN_POINT('Ctrl Pts',(83.7790221633972,0.179309719652794,4.43079803619748));
#14031=CARTESIAN_POINT('Ctrl Pts',(83.7784632959555,0.190984324241664,4.43027577732082));
#14032=CARTESIAN_POINT('Ctrl Pts',(83.77240277904,0.317587044874403,4.42461225405919));
#14033=CARTESIAN_POINT('Ctrl Pts',(83.7662160650533,0.444085919803523,4.41343834714048));
#14034=CARTESIAN_POINT('Ctrl Pts',(83.7599947286139,0.569976779683552,4.39681746005267));
#14035=CARTESIAN_POINT('Ctrl Pts',(83.7537794334196,0.695745392914888,4.38021271272073));
#14036=CARTESIAN_POINT('Ctrl Pts',(83.7475299337402,0.820907251237237,4.35817192446295));
#14037=CARTESIAN_POINT('Ctrl Pts',(83.7413201587169,0.944975540862707,4.33079772638433));
#14038=CARTESIAN_POINT('Ctrl Pts',(83.7366031774661,1.03921853578525,4.31000412619592));
#14039=CARTESIAN_POINT('Ctrl Pts',(83.7319092369034,1.13283341894311,4.28613239844926));
#14040=CARTESIAN_POINT('Ctrl Pts',(83.7273552997934,1.2255595276426,4.25908925970827));
#14041=CARTESIAN_POINT('Ctrl Pts',(83.7259184348083,1.25481660686286,4.25055656849965));
#14042=CARTESIAN_POINT('Ctrl Pts',(83.7244955076997,1.28398483229506,4.2417082638057));
#14043=CARTESIAN_POINT('Ctrl Pts',(83.7230901924276,1.31305499752794,4.23254176849106));
#14044=CARTESIAN_POINT('Ctrl Pts',(83.7181776848939,1.41467447647992,4.20049879693493));
#14045=CARTESIAN_POINT('Ctrl Pts',(83.7133888293406,1.51513881220252,4.16472052270079));
#14046=CARTESIAN_POINT('Ctrl Pts',(83.7086207664946,1.61424885826624,4.12550486535286));
#14047=CARTESIAN_POINT('Ctrl Pts',(83.7077039761991,1.6333054712653,4.11796458426871));
#14048=CARTESIAN_POINT('Ctrl Pts',(83.7067879546218,1.65231215695153,4.11029715863561));
#14049=CARTESIAN_POINT('Ctrl Pts',(83.7058719705771,1.67126769888763,4.10250461110111));
#14050=CARTESIAN_POINT('Ctrl Pts',(83.6983238768225,1.82746933638149,4.03829074218398));
#14051=CARTESIAN_POINT('Ctrl Pts',(83.6907782499507,1.98020189059388,3.96558359210025));
#14052=CARTESIAN_POINT('Ctrl Pts',(83.6832297395517,2.12854987973628,3.88482306144842));
#14053=CARTESIAN_POINT('Ctrl Pts',(83.679419412548,2.20343277968634,3.84405686858208));
#14054=CARTESIAN_POINT('Ctrl Pts',(83.6756083666427,2.27719782470252,3.80123805572656));
#14055=CARTESIAN_POINT('Ctrl Pts',(83.6717959857574,2.34972329100296,3.75641988700811));
#14056=CARTESIAN_POINT('Ctrl Pts',(83.6664177671139,2.45203673415599,3.69319380393264));
#14057=CARTESIAN_POINT('Ctrl Pts',(83.6612005502138,2.551736824447,3.62574492221054));
#14058=CARTESIAN_POINT('Ctrl Pts',(83.6562305162575,2.64830487667778,3.55415362758043));
#14059=CARTESIAN_POINT('Ctrl Pts',(83.6559476717751,2.65380056161585,3.55007936916362));
#14060=CARTESIAN_POINT('Ctrl Pts',(83.6556656278551,2.65928609232917,3.54599170401589));
#14061=CARTESIAN_POINT('Ctrl Pts',(83.6553844003821,2.66476136953762,3.54189065047767));
#14062=CARTESIAN_POINT('Ctrl Pts',(83.6501559879268,2.76655443852363,3.46564632350785));
#14063=CARTESIAN_POINT('Ctrl Pts',(83.6449872923774,2.86503315524786,3.38508292429783));
#14064=CARTESIAN_POINT('Ctrl Pts',(83.6398139617035,2.95979960583976,3.30050642057553));
#14065=CARTESIAN_POINT('Ctrl Pts',(83.6346374916142,3.05462356508098,3.21587859193324));
#14066=CARTESIAN_POINT('Ctrl Pts',(83.6294560182221,3.1457304301424,3.12723254995599));
#14067=CARTESIAN_POINT('Ctrl Pts',(83.6241890224578,3.23274317603943,3.03491436927644));
#14068=CARTESIAN_POINT('Ctrl Pts',(83.6193227826456,3.31313528326577,2.94962050797348));
#14069=CARTESIAN_POINT('Ctrl Pts',(83.6143830940161,3.39003289396152,2.86119163286796));
#14070=CARTESIAN_POINT('Ctrl Pts',(83.6092990232269,3.46315841226844,2.76993532987214));
#14071=CARTESIAN_POINT('Ctrl Pts',(83.6088724314768,3.46929419285222,2.76227824018534));
#14072=CARTESIAN_POINT('Ctrl Pts',(83.6084448232082,3.47540344518774,2.75460123514701));
#14073=CARTESIAN_POINT('Ctrl Pts',(83.6080161565174,3.48148602117807,2.74690449123667));
#14074=CARTESIAN_POINT('Ctrl Pts',(83.6055834116648,3.51600551091099,2.70322436741865));
#14075=CARTESIAN_POINT('Ctrl Pts',(83.6031165029076,3.54966513737925,2.65890943823865));
#14076=CARTESIAN_POINT('Ctrl Pts',(83.6006076436536,3.58243728965208,2.61399563943773));
#14077=CARTESIAN_POINT('Ctrl Pts',(83.6006056057948,3.58246390932781,2.6139591575262));
#14078=CARTESIAN_POINT('Ctrl Pts',(83.6006035679082,3.58249052841819,2.61392267521949));
#14079=CARTESIAN_POINT('Ctrl Pts',(83.6006015299941,3.58251714692321,2.61388619251767));
#14080=CARTESIAN_POINT('Ctrl Pts',(83.5954166817284,3.65023977746171,2.52106713544909));
#14081=CARTESIAN_POINT('Ctrl Pts',(83.5900423118012,3.71435230953212,2.42542966378751));
#14082=CARTESIAN_POINT('Ctrl Pts',(83.584555266241,3.77464845947616,2.32730368333586));
#14083=CARTESIAN_POINT('Ctrl Pts',(83.5839973965675,3.78077878828693,2.31732718358245));
#14084=CARTESIAN_POINT('Ctrl Pts',(83.5834383621824,3.78686967036942,2.30732500482146));
#14085=CARTESIAN_POINT('Ctrl Pts',(83.5828782438472,3.79292089131384,2.29729752376806));
#14086=CARTESIAN_POINT('Ctrl Pts',(83.5768163714489,3.85841014048677,2.1887752583749));
#14087=CARTESIAN_POINT('Ctrl Pts',(83.5706280763583,3.91925405413166,2.07728344318731));
#14088=CARTESIAN_POINT('Ctrl Pts',(83.5644049661865,3.97522582996733,1.96327700683015));
#14089=CARTESIAN_POINT('Ctrl Pts',(83.5581879051488,4.03114319880001,1.84938138969269));
#14090=CARTESIAN_POINT('Ctrl Pts',(83.5519364479608,4.0821982463679,1.73297617410154));
#14091=CARTESIAN_POINT('Ctrl Pts',(83.5457245712611,4.12820645876471,1.61452358162241));
#14092=CARTESIAN_POINT('Ctrl Pts',(83.5410209908633,4.16304348732034,1.52483228235841));
#14093=CARTESIAN_POINT('Ctrl Pts',(83.5363402224714,4.19498794677658,1.43396432677261));
#14094=CARTESIAN_POINT('Ctrl Pts',(83.5317995616617,4.22381742177296,1.34208276760707));
#14095=CARTESIAN_POINT('Ctrl Pts',(83.5303478472981,4.23303461827788,1.31270691577096));
#14096=CARTESIAN_POINT('Ctrl Pts',(83.5289104543474,4.24193329377069,1.28322783771989));
#14097=CARTESIAN_POINT('Ctrl Pts',(83.5274912160669,4.25050589703514,1.25365195119791));
#14098=CARTESIAN_POINT('Ctrl Pts',(83.5225652846931,4.28025992492025,1.15099914840792));
#14099=CARTESIAN_POINT('Ctrl Pts',(83.5177622460202,4.30624407429985,1.04723109347148));
#14100=CARTESIAN_POINT('Ctrl Pts',(83.5129795917191,4.3285951463578,0.942680774685479));
#14101=CARTESIAN_POINT('Ctrl Pts',(83.5120764624614,4.33281579578061,0.922938086661672));
#14102=CARTESIAN_POINT('Ctrl Pts',(83.5111740600778,4.33690692070658,0.903167357049539));
#14103=CARTESIAN_POINT('Ctrl Pts',(83.5102716943254,4.34086947147152,0.883370621573313));
#14104=CARTESIAN_POINT('Ctrl Pts',(83.5027215983376,4.37402414135265,0.71773129772002));
#14105=CARTESIAN_POINT('Ctrl Pts',(83.4951739851061,4.39818241547758,0.55026993718802));
#14106=CARTESIAN_POINT('Ctrl Pts',(83.4876235034185,4.41320306700913,0.381992895145997));
#14107=CARTESIAN_POINT('Ctrl Pts',(83.4838129798435,4.42078358294728,0.297068030432569));
#14108=CARTESIAN_POINT('Ctrl Pts',(83.4800017414153,4.42603592339558,0.211935627319798));
#14109=CARTESIAN_POINT('Ctrl Pts',(83.4761891720582,4.42893697379109,0.126726501352696));
#14110=CARTESIAN_POINT('Ctrl Pts',(83.4711900572098,4.43274088730706,0.014998643590784));
#14111=CARTESIAN_POINT('Ctrl Pts',(83.4663151445685,4.43228269129631,-0.0968724714744418));
#14112=CARTESIAN_POINT('Ctrl Pts',(83.4616590637086,4.42734101575312,-0.20850640372019));
#14113=CARTESIAN_POINT('Ctrl Pts',(83.4610199200294,4.42666266827954,-0.223830476545876));
#14114=CARTESIAN_POINT('Ctrl Pts',(83.4603848998537,4.42589984630004,-0.239150000201453));
#14115=CARTESIAN_POINT('Ctrl Pts',(83.4597542479529,4.42505198770308,-0.254463914514458));
#14116=CARTESIAN_POINT('Ctrl Pts',(83.4545238336106,4.41802013421873,-0.381472359208858));
#14117=CARTESIAN_POINT('Ctrl Pts',(83.4493532883236,4.40555445277623,-0.508116824523829));
#14118=CARTESIAN_POINT('Ctrl Pts',(83.4441783208528,4.38768895006725,-0.633896375290781));
#14119=CARTESIAN_POINT('Ctrl Pts',(83.4390002249744,4.36981264717916,-0.759751963194735));
#14120=CARTESIAN_POINT('Ctrl Pts',(83.4338173390892,4.34652961734655,-0.884741454493317));
#14121=CARTESIAN_POINT('Ctrl Pts',(83.4285492038077,4.31791882352173,-1.00835906006262));
#14122=CARTESIAN_POINT('Ctrl Pts',(83.4236813525029,4.29148193786622,-1.12258394048542));
#14123=CARTESIAN_POINT('Ctrl Pts',(83.4187402686918,4.2604959670513,-1.23563797592087));
#14124=CARTESIAN_POINT('Ctrl Pts',(83.4136550391749,4.22506300672305,-1.34711935625403));
#14125=CARTESIAN_POINT('Ctrl Pts',(83.413229011399,4.22209452216738,-1.35645898671952));
#14126=CARTESIAN_POINT('Ctrl Pts',(83.4128019719122,4.21909483432159,-1.36578760828526));
#14127=CARTESIAN_POINT('Ctrl Pts',(83.4123738790171,4.21606400765798,-1.37510500073172));
#14128=CARTESIAN_POINT('Ctrl Pts',(83.4099529500042,4.19892423195254,-1.42779624124671));
#14129=CARTESIAN_POINT('Ctrl Pts',(83.4074982579746,4.18078900305616,-1.48012728715261));
#14130=CARTESIAN_POINT('Ctrl Pts',(83.4050021356873,4.16167269623072,-1.53205585686474));
#14131=CARTESIAN_POINT('Ctrl Pts',(83.4050001147405,4.16165721900856,-1.53209790002805));
#14132=CARTESIAN_POINT('Ctrl Pts',(83.4049980937665,4.16164174114336,-1.5321399429277));
#14133=CARTESIAN_POINT('Ctrl Pts',(83.4049960727654,4.16162626263514,-1.53218198556367));
#14134=CARTESIAN_POINT('Ctrl Pts',(83.3998090342966,4.12189960606499,-1.6400873041627));
#14135=CARTESIAN_POINT('Ctrl Pts',(83.39443278481,4.07781980193203,-1.74654803110892));
#14136=CARTESIAN_POINT('Ctrl Pts',(83.3889442402674,4.0295474499751,-1.85120901823054));
#14137=CARTESIAN_POINT('Ctrl Pts',(83.3883887623086,4.02466196033003,-1.86180142046694));
#14138=CARTESIAN_POINT('Ctrl Pts',(83.3878321341325,4.01973356519352,-1.87237536606769));
#14139=CARTESIAN_POINT('Ctrl Pts',(83.3872744354734,4.01476245694717,-1.88293047238602));
#14140=CARTESIAN_POINT('Ctrl Pts',(83.3812136369893,3.96073886404263,-1.99763824750323));
#14141=CARTESIAN_POINT('Ctrl Pts',(83.3750269467086,3.90166577113011,-2.11012439295221));
#14142=CARTESIAN_POINT('Ctrl Pts',(83.3688058702781,3.83779625481318,-2.21994776795051));
#14143=CARTESIAN_POINT('Ctrl Pts',(83.3625908230251,3.77398863785629,-2.32966470724957));
#14144=CARTESIAN_POINT('Ctrl Pts',(83.3563418066165,3.70539419617667,-2.43672425023083));
#14145=CARTESIAN_POINT('Ctrl Pts',(83.3501326438124,3.6322954950446,-2.54071638406537));
#14146=CARTESIAN_POINT('Ctrl Pts',(83.3453747546907,3.57628222467187,-2.6204023349633));
#14147=CARTESIAN_POINT('Ctrl Pts',(83.3406403877156,3.51762241240995,-2.69828955358027));
#14148=CARTESIAN_POINT('Ctrl Pts',(83.3360454945849,3.45633625635999,-2.77409862803806));
#14149=CARTESIAN_POINT('Ctrl Pts',(83.3346482625727,3.43770013649747,-2.79715093037385));
#14150=CARTESIAN_POINT('Ctrl Pts',(83.3332639272723,3.41882139867615,-2.82001079176768));
#14151=CARTESIAN_POINT('Ctrl Pts',(83.3318957489754,3.39970124785076,-2.84266964208191));
#14152=CARTESIAN_POINT('Ctrl Pts',(83.3270132673139,3.33146906935275,-2.92353002510502));
#14153=CARTESIAN_POINT('Ctrl Pts',(83.3222563202797,3.26027188291528,-3.00191668634912));
#14154=CARTESIAN_POINT('Ctrl Pts',(83.3175212277932,3.18645817129212,-3.07776470819284));
#14155=CARTESIAN_POINT('Ctrl Pts',(83.3165680478573,3.17159938044212,-3.09303300818994));
#14156=CARTESIAN_POINT('Ctrl Pts',(83.3156157535154,3.15663444020069,-3.10819855383837));
#14157=CARTESIAN_POINT('Ctrl Pts',(83.314663499032,3.14156600359999,-3.12326098650216));
#14158=CARTESIAN_POINT('Ctrl Pts',(83.3071167037327,3.02214581867496,-3.24263358910162));
#14159=CARTESIAN_POINT('Ctrl Pts',(83.2995723295983,2.89622647997022,-3.35553454280886));
#14160=CARTESIAN_POINT('Ctrl Pts',(83.2920250328264,2.76456537085735,-3.46128825066738));
#14161=CARTESIAN_POINT('Ctrl Pts',(83.2882075858386,2.69797075830039,-3.51477881632305));
#14162=CARTESIAN_POINT('Ctrl Pts',(83.2843894074362,2.62990689191812,-3.56644000015238));
#14163=CARTESIAN_POINT('Ctrl Pts',(83.2805698800677,2.56047027845926,-3.61617938269018));
#14164=CARTESIAN_POINT('Ctrl Pts',(83.274882611746,2.45707930517862,-3.69024122002343));
#14165=CARTESIAN_POINT('Ctrl Pts',(83.2694212546832,2.35041368498791,-3.75971890711027));
#14166=CARTESIAN_POINT('Ctrl Pts',(83.2641962605888,2.24088491821295,-3.82421505258511));
#14167=CARTESIAN_POINT('Ctrl Pts',(83.2589657305283,2.13124010393381,-3.88877953277175));
#14168=CARTESIAN_POINT('Ctrl Pts',(83.2537941812851,2.0188842603045,-3.94861631443767));
#14169=CARTESIAN_POINT('Ctrl Pts',(83.2486170992431,1.90425347118074,-4.00347568986756));
#14170=CARTESIAN_POINT('Ctrl Pts',(83.2434368894082,1.78955342656573,-4.05836820921127));
#14171=CARTESIAN_POINT('Ctrl Pts',(83.2382507755029,1.67257559122187,-4.10827691655245));
#14172=CARTESIAN_POINT('Ctrl Pts',(83.232978127041,1.55378509690204,-4.15298685851507));
#14173=CARTESIAN_POINT('Ctrl Pts',(83.2281105165493,1.44411993324624,-4.19426224111572));
#14174=CARTESIAN_POINT('Ctrl Pts',(83.2231687085409,1.33290939295841,-4.23110701948943));
#14175=CARTESIAN_POINT('Ctrl Pts',(83.2180819163818,1.22054383348356,-4.2633835944284));
#14176=CARTESIAN_POINT('Ctrl Pts',(83.2176507811159,1.21102019779215,-4.26611922216453));
#14177=CARTESIAN_POINT('Ctrl Pts',(83.2172186043491,1.20148824518652,-4.26882205787307));
#14178=CARTESIAN_POINT('Ctrl Pts',(83.2167853429832,1.19194820207161,-4.27149203085028));
#14179=CARTESIAN_POINT('Ctrl Pts',(83.2143813551094,1.13901445406698,-4.28630660506678));
#14180=CARTESIAN_POINT('Ctrl Pts',(83.2119439043162,1.08583272356488,-4.3001091693648));
#14181=CARTESIAN_POINT('Ctrl Pts',(83.2094655122813,1.032445146656,-4.31288851184167));
#14182=CARTESIAN_POINT('Ctrl Pts',(83.2094634559398,1.03240085056045,-4.31289911496338));
#14183=CARTESIAN_POINT('Ctrl Pts',(83.2094613995701,1.03235655432311,-4.31290971738082));
#14184=CARTESIAN_POINT('Ctrl Pts',(83.2094593431722,1.03231225794397,-4.31292031909402));
#14185=CARTESIAN_POINT('Ctrl Pts',(83.2042762343558,0.920664139950302,-4.33964172047668));
#14186=CARTESIAN_POINT('Ctrl Pts',(83.1989037007853,0.807805603682432,-4.36195383867267));
#14187=CARTESIAN_POINT('Ctrl Pts',(83.1934186670854,0.694120027050924,-4.37979314581744));
#14188=CARTESIAN_POINT('Ctrl Pts',(83.1928629297045,0.682601533626714,-4.38160060414353));
#14189=CARTESIAN_POINT('Ctrl Pts',(83.1923060374522,0.671074589850501,-4.3833621661427));
#14190=CARTESIAN_POINT('Ctrl Pts',(83.1917480703369,0.659539620962272,-4.38507777932936));
#14191=CARTESIAN_POINT('Ctrl Pts',(83.1856904731488,0.534309668887365,-4.40370341752789));
#14192=CARTESIAN_POINT('Ctrl Pts',(83.1795067222463,0.408128309738017,-4.4169110341505));
#14193=CARTESIAN_POINT('Ctrl Pts',(83.1732884166176,0.281501608649066,-4.42466627281055));
#14194=CARTESIAN_POINT('Ctrl Pts',(83.1670761523311,0.154997930659677,-4.43241397693414));
#14195=CARTESIAN_POINT('Ctrl Pts',(83.1608297506867,0.0280497684847077,
-4.43472026555932));
#14196=CARTESIAN_POINT('Ctrl Pts',(83.1546231847352,-0.0988462957672127,
-4.43159260547438));
#14197=CARTESIAN_POINT('Ctrl Pts',(83.1499306446216,-0.194787413032101,
-4.42922790484522));
#14198=CARTESIAN_POINT('Ctrl Pts',(83.1452609940217,-0.290701728684633,
-4.42375682800405));
#14199=CARTESIAN_POINT('Ctrl Pts',(83.1407318165524,-0.386354485368013,
-4.41503603971653));
#14200=CARTESIAN_POINT('Ctrl Pts',(83.1392748197715,-0.417125140640413,
-4.41223063839405));
#14201=CARTESIAN_POINT('Ctrl Pts',(83.1378323598895,-0.447868327306429,
-4.40908898022418));
#14202=CARTESIAN_POINT('Ctrl Pts',(83.1364083513007,-0.478575093763186,
-4.40560645526888));
#14203=CARTESIAN_POINT('Ctrl Pts',(83.1314823913209,-0.584796575758634,
-4.39355963287357));
#14204=CARTESIAN_POINT('Ctrl Pts',(83.1266791266776,-0.690596500927511,
-4.37760349242614));
#14205=CARTESIAN_POINT('Ctrl Pts',(83.1218960858815,-0.795719867644331,
-4.35799264321106));
#14206=CARTESIAN_POINT('Ctrl Pts',(83.1210003234424,-0.815407252174682,
-4.35431994567937));
#14207=CARTESIAN_POINT('Ctrl Pts',(83.1201052703218,-0.835071050871667,
-4.35051903223484));
#14208=CARTESIAN_POINT('Ctrl Pts',(83.1192102534356,-0.854709785325135,
-4.34659152404242));
#14209=CARTESIAN_POINT('Ctrl Pts',(83.1116643988368,-1.02028323648516,-4.31347884626688));
#14210=CARTESIAN_POINT('Ctrl Pts',(83.1041210386046,-1.18407820825324,-4.2713714180056));
#14211=CARTESIAN_POINT('Ctrl Pts',(83.0965748157052,-1.34511223604663,-4.22052663331527));
#14212=CARTESIAN_POINT('Ctrl Pts',(83.0927737523542,-1.42622573474487,-4.19491590722648));
#14213=CARTESIAN_POINT('Ctrl Pts',(83.0889719781047,-1.50663820973591,-4.16708763564311));
#14214=CARTESIAN_POINT('Ctrl Pts',(83.0851688787083,-1.58622088491304,-4.13707070931025));
#14215=CARTESIAN_POINT('Ctrl Pts',(83.0802290600159,-1.68959025432714,-4.09808193769794));
#14216=CARTESIAN_POINT('Ctrl Pts',(83.0754089626005,-1.79148850189328,-4.05520097269121));
#14217=CARTESIAN_POINT('Ctrl Pts',(83.0708045781324,-1.89149125190055,-4.00836457291793));
#14218=CARTESIAN_POINT('Ctrl Pts',(83.0701160143723,-1.9064461867097,-4.00136041247981));
#14219=CARTESIAN_POINT('Ctrl Pts',(83.0694322747687,-1.92135864759915,-3.99426783906397));
#14220=CARTESIAN_POINT('Ctrl Pts',(83.0687536803555,-1.93622712847732,-3.98708669161156));
#14221=CARTESIAN_POINT('Ctrl Pts',(83.0635317258871,-2.05064382372104,-3.93182595809779));
#14222=CARTESIAN_POINT('Ctrl Pts',(83.0583701263716,-2.16263885447323,-3.8717010322688));
#14223=CARTESIAN_POINT('Ctrl Pts',(83.0532046183295,-2.27176411047279,-3.80693589126885));
#14224=CARTESIAN_POINT('Ctrl Pts',(83.0480359361002,-2.38095642357315,-3.74213095230876));
#14225=CARTESIAN_POINT('Ctrl Pts',(83.0428629803953,-2.48727516552271,-3.67267980234581));
#14226=CARTESIAN_POINT('Ctrl Pts',(83.0376052600746,-2.5902850983655,-3.5988496773313));
#14227=CARTESIAN_POINT('Ctrl Pts',(83.0327438048167,-2.68553135512561,-3.53058399799632));
#14228=CARTESIAN_POINT('Ctrl Pts',(83.0278094365958,-2.77794913347238,-3.45857417713402));
#14229=CARTESIAN_POINT('Ctrl Pts',(83.022730999609,-2.86720719965072,-3.38306923522428));
#14230=CARTESIAN_POINT('Ctrl Pts',(83.0223090528177,-2.87462329139591,-3.37679583495479));
#14231=CARTESIAN_POINT('Ctrl Pts',(83.02188611148,-2.88201760041316,-3.37049830368306));
#14232=CARTESIAN_POINT('Ctrl Pts',(83.0214621347834,-2.88938995281641,-3.3641767821702));
#14233=CARTESIAN_POINT('Ctrl Pts',(83.0189708446667,-2.932709948522,-3.32703147632875));
#14234=CARTESIAN_POINT('Ctrl Pts',(83.0164437251978,-2.97527093498445,-3.2890586609128));
#14235=CARTESIAN_POINT('Ctrl Pts',(83.0138723507173,-3.01703632090005,-3.2502907069457));
#14236=CARTESIAN_POINT('Ctrl Pts',(83.0138703039779,-3.01706956493473,-3.25025984877983));
#14237=CARTESIAN_POINT('Ctrl Pts',(83.0138682572104,-3.01710280846552,-3.25022899011018));
#14238=CARTESIAN_POINT('Ctrl Pts',(83.0138662104149,-3.01713605149244,-3.25019813093678));
#14239=CARTESIAN_POINT('Ctrl Pts',(83.0087347594115,-3.1004785067607,-3.17283215325411));
#14240=CARTESIAN_POINT('Ctrl Pts',(83.0034159680191,-3.18089387926395,-3.09206394837344));
#14241=CARTESIAN_POINT('Ctrl Pts',(82.9979843348117,-3.25811675623012,-3.00817024856034));
#14242=CARTESIAN_POINT('Ctrl Pts',(82.9974493435073,-3.26572286034265,-2.99990709856862));
#14243=CARTESIAN_POINT('Ctrl Pts',(82.996913257484,-3.27329798884271,-2.99161366854329));
#14244=CARTESIAN_POINT('Ctrl Pts',(82.996376147928,-3.28084188596267,-2.98329025010284));
#14245=CARTESIAN_POINT('Ctrl Pts',(82.99039332449,-3.3648727954933,-2.8905763104994));
#14246=CARTESIAN_POINT('Ctrl Pts',(82.9842840229385,-3.44502954170072,-2.79413572203119));
#14247=CARTESIAN_POINT('Ctrl Pts',(82.9781369279056,-3.5210052932334,-2.6943596675154));
#14248=CARTESIAN_POINT('Ctrl Pts',(82.9719965698146,-3.59689777873267,-2.59469296310303));
#14249=CARTESIAN_POINT('Ctrl Pts',(82.9658188451291,-3.66861870715653,-2.4916983245184));
#14250=CARTESIAN_POINT('Ctrl Pts',(82.9596760395827,-3.73590152906811,-2.3857833174973));
#14251=CARTESIAN_POINT('Ctrl Pts',(82.9549408128507,-3.787766986067,-2.30413795711975));
#14252=CARTESIAN_POINT('Ctrl Pts',(82.9502264590364,-3.83699676504752,-2.22075475036848));
#14253=CARTESIAN_POINT('Ctrl Pts',(82.9456496772315,-3.88334000890611,-2.13575781248512));
#14254=CARTESIAN_POINT('Ctrl Pts',(82.944292813768,-3.8970792381408,-2.11055904958906));
#14255=CARTESIAN_POINT('Ctrl Pts',(82.942948041854,-3.91056460553878,-2.08521876279161));
#14256=CARTESIAN_POINT('Ctrl Pts',(82.9416184023416,-3.92378920759747,-2.05974098750738));
#14257=CARTESIAN_POINT('Ctrl Pts',(82.9368771085923,-3.97094614186146,-1.9688910875301));
#14258=CARTESIAN_POINT('Ctrl Pts',(82.9322682646822,-4.01487748023783,-1.87634492024307));
#14259=CARTESIAN_POINT('Ctrl Pts',(82.9276849638517,-4.05566876559709,-1.78243544837345));
#14260=CARTESIAN_POINT('Ctrl Pts',(82.9266495030548,-4.06488434589737,-1.76121939030247));
#14261=CARTESIAN_POINT('Ctrl Pts',(82.9256153459765,-4.07393974301493,-1.73993355659287));
#14262=CARTESIAN_POINT('Ctrl Pts',(82.924581259878,-4.08283608159913,-1.71858144525149));
#14263=CARTESIAN_POINT('Ctrl Pts',(82.9166349033586,-4.15119932350881,-1.55450275837398));
#14264=CARTESIAN_POINT('Ctrl Pts',(82.9086926499015,-4.21017510191321,-1.38650973643088));
#14265=CARTESIAN_POINT('Ctrl Pts',(82.900749320533,-4.25938512909566,-1.21574718217419));
#14266=CARTESIAN_POINT('Ctrl Pts',(82.8974727757882,-4.27968377824818,-1.14530931867953));
#14267=CARTESIAN_POINT('Ctrl Pts',(82.8941960587482,-4.29832015049098,-1.07440021001745));
#14268=CARTESIAN_POINT('Ctrl Pts',(82.890918840253,-4.31526507376258,-1.00310021346923));
#14269=CARTESIAN_POINT('Ctrl Pts',(82.8870928818563,-4.33504726758591,-0.919861692484912));
#14270=CARTESIAN_POINT('Ctrl Pts',(82.8832662196026,-4.35252498261166,-0.836085699931758));
#14271=CARTESIAN_POINT('Ctrl Pts',(82.8795678067457,-4.36742592605661,-0.75188043808983));
#14272=CARTESIAN_POINT('Ctrl Pts',(82.8778392658581,-4.37439023507361,-0.712525113610447));
#14273=CARTESIAN_POINT('Ctrl Pts',(82.8761387395344,-4.38079153195561,-0.67307674815633));
#14274=CARTESIAN_POINT('Ctrl Pts',(82.874479392903,-4.38660146132129,-0.633550254867047));
#14275=CARTESIAN_POINT('Ctrl Pts',(82.8692639398317,-4.40486251261772,-0.509315470570285));
#14276=CARTESIAN_POINT('Ctrl Pts',(82.8641471892087,-4.41780787734669,-0.384390475029427));
#14277=CARTESIAN_POINT('Ctrl Pts',(82.8590372507684,-4.4254380234901,-0.25927381989085));
#14278=CARTESIAN_POINT('Ctrl Pts',(82.8554668444273,-4.43076934450161,-0.171852551688031));
#14279=CARTESIAN_POINT('Ctrl Pts',(82.8518993357656,-4.43350664674304,-0.0843371748317401));
#14280=CARTESIAN_POINT('Ctrl Pts',(82.8483099710866,-4.43364346784954,0.00310368774768347));
#14281=CARTESIAN_POINT('Ctrl Pts',(90.1028989154209,-1.84736391785682,1.20202435615052));
#14282=CARTESIAN_POINT('Ctrl Pts',(90.140690073821,-2.22792678283258,0.617153363646938));
#14283=CARTESIAN_POINT('Ctrl Pts',(90.2162692554159,-2.38778162526882,-0.933200414266254));
#14284=CARTESIAN_POINT('Ctrl Pts',(90.3296364602056,-0.62872205324772,-2.48534112021196));
#14285=CARTESIAN_POINT('Ctrl Pts',(90.4052125065953,0.88959187531312,-2.13379067845246));
#14286=CARTESIAN_POINT('Ctrl Pts',(90.4430005297901,1.42252785196827,-1.68345790276281));
#14287=CARTESIAN_POINT('Ctrl Pts',(90.1853507684723,-1.72766177787012,1.12413775981909));
#14288=CARTESIAN_POINT('Ctrl Pts',(90.2231419268724,-2.08356561984736,0.577164178184089));
#14289=CARTESIAN_POINT('Ctrl Pts',(90.2987211084673,-2.23306247783782,-0.872732584650031));
#14290=CARTESIAN_POINT('Ctrl Pts',(90.4120883132569,-0.587983260796952,
-2.32430048939166));
#14291=CARTESIAN_POINT('Ctrl Pts',(90.4876643596466,0.831949712791466,-1.99552917619753));
#14292=CARTESIAN_POINT('Ctrl Pts',(90.5254523828415,1.33035346963605,-1.5743762477676));
#14293=CARTESIAN_POINT('Ctrl Pts',(90.2678026215237,-1.60795963788343,1.04625116348766));
#14294=CARTESIAN_POINT('Ctrl Pts',(90.3055937799238,-1.93920445686214,0.537174992721241));
#14295=CARTESIAN_POINT('Ctrl Pts',(90.3811729615186,-2.07834333040681,-0.812264755033806));
#14296=CARTESIAN_POINT('Ctrl Pts',(90.4945401663084,-0.547244468346182,
-2.16325985857137));
#14297=CARTESIAN_POINT('Ctrl Pts',(90.5701162126981,0.774307550269809,-1.85726767394259));
#14298=CARTESIAN_POINT('Ctrl Pts',(90.6079042358929,1.23817908730384,-1.4652945927724));
#14299=CARTESIAN_POINT('Ctrl Pts',(90.3502544745751,-1.48825749789673,0.968364567156219));
#14300=CARTESIAN_POINT('Ctrl Pts',(90.3880456329751,-1.79484329387692,0.497185807258393));
#14301=CARTESIAN_POINT('Ctrl Pts',(90.4636248145701,-1.92362418297579,-0.751796925417581));
#14302=CARTESIAN_POINT('Ctrl Pts',(90.5769920193598,-0.506505675895414,
-2.00221922775108));
#14303=CARTESIAN_POINT('Ctrl Pts',(90.6525680657495,0.716665387748153,-1.71900617168766));
#14304=CARTESIAN_POINT('Ctrl Pts',(90.6903560889443,1.14600470497162,-1.35621293777719));
#14305=CARTESIAN_POINT('',(90.4430005297901,1.42252785196811,-1.68345790276294));
#14306=CARTESIAN_POINT('',(90.4431198242969,-1.73942095919881,-0.360857735792951));
#14307=CARTESIAN_POINT('Ctrl Pts',(90.4430005297901,1.4225278519681,-1.68345790276293));
#14308=CARTESIAN_POINT('Ctrl Pts',(90.4430005297901,1.35849356753145,-1.72802743598216));
#14309=CARTESIAN_POINT('Ctrl Pts',(90.4430005297901,1.29211327677423,-1.76879332847206));
#14310=CARTESIAN_POINT('Ctrl Pts',(90.4430005297901,1.2237535666043,-1.80575874571065));
#14311=CARTESIAN_POINT('Ctrl Pts',(90.4430005297901,1.15444662534627,-1.8432363768294));
#14312=CARTESIAN_POINT('Ctrl Pts',(90.4430005297901,1.08310399459898,-1.87680762783793));
#14313=CARTESIAN_POINT('Ctrl Pts',(90.4430005297901,1.01008882139701,-1.90642508440335));
#14314=CARTESIAN_POINT('Ctrl Pts',(90.4430005297901,0.937375387724121,-1.93592014507482));
#14315=CARTESIAN_POINT('Ctrl Pts',(90.4430005297901,0.863002156179472,-1.96149402884287));
#14316=CARTESIAN_POINT('Ctrl Pts',(90.4430005297901,0.787324930454048,-1.98304902265781));
#14317=CARTESIAN_POINT('Ctrl Pts',(90.4430005297901,0.744830143839778,-1.99515272828203));
#14318=CARTESIAN_POINT('Ctrl Pts',(90.4430005297901,0.701924229092549,-2.00598831162974));
#14319=CARTESIAN_POINT('Ctrl Pts',(90.4430005297901,0.658671653783688,-2.0155313726465));
#14320=CARTESIAN_POINT('Ctrl Pts',(90.4430005297901,0.646172907588059,-2.01828904191188));
#14321=CARTESIAN_POINT('Ctrl Pts',(90.4430005297901,0.633654218360874,-2.02093674442495));
#14322=CARTESIAN_POINT('Ctrl Pts',(90.4430005297901,0.6211203149044,-2.02347372260162));
#14323=CARTESIAN_POINT('Ctrl Pts',(90.4430005297901,0.54560059660241,-2.03875961321869));
#14324=CARTESIAN_POINT('Ctrl Pts',(90.4430005297901,0.469491648693074,-2.05003826325601));
#14325=CARTESIAN_POINT('Ctrl Pts',(90.4430005297901,0.393135312105228,-2.05726598238489));
#14326=CARTESIAN_POINT('Ctrl Pts',(90.4430005297901,0.317994445888144,-2.06437864782154));
#14327=CARTESIAN_POINT('Ctrl Pts',(90.4430005297901,0.242613051580121,-2.06756819235657));
#14328=CARTESIAN_POINT('Ctrl Pts',(90.4430005297901,0.167322657815908,-2.06674371029539));
#14329=CARTESIAN_POINT('Ctrl Pts',(90.4430005297901,0.11103882258771,-2.06612736324021));
#14330=CARTESIAN_POINT('Ctrl Pts',(90.4430005297901,0.0548058830603974,
-2.06326681098423));
#14331=CARTESIAN_POINT('Ctrl Pts',(90.4430005297901,-0.0012308310801181,
-2.05810621712317));
#14332=CARTESIAN_POINT('Ctrl Pts',(90.4430005297901,-0.0254665698698789,
-2.0558742731783));
#14333=CARTESIAN_POINT('Ctrl Pts',(90.4430005297901,-0.0496655066289054,
-2.05321190325344));
#14334=CARTESIAN_POINT('Ctrl Pts',(90.4430005297901,-0.0738153724767166,
-2.05011370335278));
#14335=CARTESIAN_POINT('Ctrl Pts',(90.4430005297901,-0.0915898373131206,
-2.04783340724109));
#14336=CARTESIAN_POINT('Ctrl Pts',(90.4430005297901,-0.109337713577792,
-2.04531700834963));
#14337=CARTESIAN_POINT('Ctrl Pts',(90.4430005297901,-0.127053980826188,
-2.04256216657338));
#14338=CARTESIAN_POINT('Ctrl Pts',(90.4430005297901,-0.141731501026049,
-2.04027984348288));
#14339=CARTESIAN_POINT('Ctrl Pts',(90.4430005297901,-0.15638983983332,-2.03783328837979));
#14340=CARTESIAN_POINT('Ctrl Pts',(90.4430005297901,-0.171003090990926,
-2.03522554868848));
#14341=CARTESIAN_POINT('Ctrl Pts',(90.4430005297901,-0.24257684235259,-2.02245318815976));
#14342=CARTESIAN_POINT('Ctrl Pts',(90.4430005297901,-0.313187615395152,
-2.00580133374315));
#14343=CARTESIAN_POINT('Ctrl Pts',(90.4430005297901,-0.382533842296712,
-1.9851947537543));
#14344=CARTESIAN_POINT('Ctrl Pts',(90.4430005297901,-0.420076293430716,
-1.97403882564059));
#14345=CARTESIAN_POINT('Ctrl Pts',(90.4430005297901,-0.457247853160685,
-1.96172298204888));
#14346=CARTESIAN_POINT('Ctrl Pts',(90.4430005297901,-0.493997977180851,
-1.94822944989876));
#14347=CARTESIAN_POINT('Ctrl Pts',(90.4430005297901,-0.563441751326172,
-1.92273179991692));
#14348=CARTESIAN_POINT('Ctrl Pts',(90.4430005297901,-0.631383008819566,
-1.8930310143353));
#14349=CARTESIAN_POINT('Ctrl Pts',(90.4430005297901,-0.697549630883036,
-1.85938942474586));
#14350=CARTESIAN_POINT('Ctrl Pts',(90.4430005297901,-0.728482655927117,
-1.84366191590772));
#14351=CARTESIAN_POINT('Ctrl Pts',(90.4430005297901,-0.759027301901942,
-1.82707257186965));
#14352=CARTESIAN_POINT('Ctrl Pts',(90.4430005297901,-0.78915271119639,-1.80964576389469));
#14353=CARTESIAN_POINT('Ctrl Pts',(90.4430005297901,-0.805665241648411,
-1.80009367135529));
#14354=CARTESIAN_POINT('Ctrl Pts',(90.4430005297901,-0.822051778690114,
-1.79028994553458));
#14355=CARTESIAN_POINT('Ctrl Pts',(90.4430005297901,-0.838306956091599,
-1.78023844910885));
#14356=CARTESIAN_POINT('Ctrl Pts',(90.4430005297901,-0.848486765356274,
-1.77394369674095));
#14357=CARTESIAN_POINT('Ctrl Pts',(90.4430005297901,-0.858617377556742,
-1.76755026518769));
#14358=CARTESIAN_POINT('Ctrl Pts',(90.4430005297901,-0.8686896401472,-1.76106412386972));
#14359=CARTESIAN_POINT('Ctrl Pts',(90.4430005297901,-0.929536413808207,
-1.72188119261045));
#14360=CARTESIAN_POINT('Ctrl Pts',(90.4430005297901,-0.988126176715454,
-1.67940471375811));
#14361=CARTESIAN_POINT('Ctrl Pts',(90.4430005297901,-1.04423185300513,-1.63391216703375));
#14362=CARTESIAN_POINT('Ctrl Pts',(90.4430005297901,-1.10035200605041,-1.58840788202328));
#14363=CARTESIAN_POINT('Ctrl Pts',(90.4430005297901,-1.15398744655177,-1.53988505913721));
#14364=CARTESIAN_POINT('Ctrl Pts',(90.4430005297901,-1.20487106311036,-1.4885881496131));
#14365=CARTESIAN_POINT('Ctrl Pts',(90.4430005297901,-1.25462208740418,-1.43843303162944));
#14366=CARTESIAN_POINT('Ctrl Pts',(90.4430005297901,-1.30174284252823,-1.38562506083014));
#14367=CARTESIAN_POINT('Ctrl Pts',(90.4430005297901,-1.34593792591377,-1.33037435808501));
#14368=CARTESIAN_POINT('Ctrl Pts',(90.4430005297901,-1.36324169050299,-1.30874197094025));
#14369=CARTESIAN_POINT('Ctrl Pts',(90.4430005297901,-1.38009642305358,-1.28673498876761));
#14370=CARTESIAN_POINT('Ctrl Pts',(90.4430005297901,-1.39648221326538,-1.26436566883624));
#14371=CARTESIAN_POINT('Ctrl Pts',(90.4430005297901,-1.40413618854343,-1.25391672377295));
#14372=CARTESIAN_POINT('Ctrl Pts',(90.4430005297901,-1.41168748957158,-1.24338902200559));
#14373=CARTESIAN_POINT('Ctrl Pts',(90.4430005297901,-1.41912637484514,-1.23279517460321));
#14374=CARTESIAN_POINT('Ctrl Pts',(90.4430005297901,-1.45875449510071,-1.17636007130585));
#14375=CARTESIAN_POINT('Ctrl Pts',(90.4430005297901,-1.49525634166903,-1.11796797580369));
#14376=CARTESIAN_POINT('Ctrl Pts',(90.4430005297901,-1.52837656473234,-1.05783238657755));
#14377=CARTESIAN_POINT('Ctrl Pts',(90.4430005297901,-1.56117405481083,-0.998282775838562));
#14378=CARTESIAN_POINT('Ctrl Pts',(90.4430005297902,-1.59065591048659,-0.937022733178418));
#14379=CARTESIAN_POINT('Ctrl Pts',(90.4430005297902,-1.61652448547098,-0.874251203149225));
#14380=CARTESIAN_POINT('Ctrl Pts',(90.4430005297902,-1.62298306524412,-0.85857910159664));
#14381=CARTESIAN_POINT('Ctrl Pts',(90.4430005297902,-1.62921615191981,-0.842812771601475));
#14382=CARTESIAN_POINT('Ctrl Pts',(90.4430005297902,-1.63521857834343,-0.826955310014817));
#14383=CARTESIAN_POINT('Ctrl Pts',(90.4430005297902,-1.64047153672403,-0.813077824501798));
#14384=CARTESIAN_POINT('Ctrl Pts',(90.4430005297902,-1.64554478527697,-0.799138477894344));
#14385=CARTESIAN_POINT('Ctrl Pts',(90.4430005297902,-1.65043379611912,-0.785144399166612));
#14386=CARTESIAN_POINT('Ctrl Pts',(90.4430005297902,-1.66472446959869,-0.744239435728744));
#14387=CARTESIAN_POINT('Ctrl Pts',(90.4430005297902,-1.67744682205688,-0.702853420185191));
#14388=CARTESIAN_POINT('Ctrl Pts',(90.4430005297902,-1.68852852013358,-0.66104002889664));
#14389=CARTESIAN_POINT('Ctrl Pts',(90.4430005297902,-1.70605020045957,-0.594927338365569));
#14390=CARTESIAN_POINT('Ctrl Pts',(90.4430005297902,-1.71947262347401,-0.527745396084227));
#14391=CARTESIAN_POINT('Ctrl Pts',(90.4430005297902,-1.72885247363525,-0.459849352265223));
#14392=CARTESIAN_POINT('Ctrl Pts',(90.4430005297902,-1.73338742826583,-0.427023083932308));
#14393=CARTESIAN_POINT('Ctrl Pts',(90.4430005297902,-1.73697664884795,-0.394030018123096));
#14394=CARTESIAN_POINT('Ctrl Pts',(90.4430005297902,-1.73962237473191,-0.360911589357311));
#14395=CARTESIAN_POINT('',(90.3498698986824,-0.176530238082941,-2.19735656904503));
#14396=CARTESIAN_POINT('Ctrl Pts',(90.4430005297901,1.42252785196811,-1.68345790276294));
#14397=CARTESIAN_POINT('Ctrl Pts',(90.4119569860875,0.984711319553738,-2.05341441334118));
#14398=CARTESIAN_POINT('Ctrl Pts',(90.380913442385,0.394220067868452,-2.23807424546201));
#14399=CARTESIAN_POINT('Ctrl Pts',(90.3498698986824,-0.175612058744845,
-2.19751079506226));
#14400=CARTESIAN_POINT('',(90.3498698986825,-1.48890580190326,0.968619417293912));
#14401=CARTESIAN_POINT('Ctrl Pts',(90.3498698986825,-0.181591443149775,
-2.19650644155093));
#14402=CARTESIAN_POINT('Ctrl Pts',(90.3498698986824,-0.257547497917167,
-2.18363784310908));
#14403=CARTESIAN_POINT('Ctrl Pts',(90.3498698986824,-0.332599118530173,
-2.16671926797208));
#14404=CARTESIAN_POINT('Ctrl Pts',(90.3498698986824,-0.406428811432403,
-2.1456565302238));
#14405=CARTESIAN_POINT('Ctrl Pts',(90.3498698986824,-0.449282745765014,
-2.1334308098551));
#14406=CARTESIAN_POINT('Ctrl Pts',(90.3498698986825,-0.491724687026784,
-2.1198079884639));
#14407=CARTESIAN_POINT('Ctrl Pts',(90.3498698986825,-0.533688867832701,
-2.10476240272968));
#14408=CARTESIAN_POINT('Ctrl Pts',(90.3498698986825,-0.572294897306717,
-2.09092082843575));
#14409=CARTESIAN_POINT('Ctrl Pts',(90.3498698986825,-0.610496552067535,
-2.07587494667672));
#14410=CARTESIAN_POINT('Ctrl Pts',(90.3498698986825,-0.648253856041698,
-2.05966215463175));
#14411=CARTESIAN_POINT('Ctrl Pts',(90.3498698986825,-0.670857500514945,
-2.04995626600279));
#14412=CARTESIAN_POINT('Ctrl Pts',(90.3498698986824,-0.693301845759945,
-2.03983211447536));
#14413=CARTESIAN_POINT('Ctrl Pts',(90.3498698986824,-0.715577834954405,
-2.0292972875901));
#14414=CARTESIAN_POINT('Ctrl Pts',(90.3498698986824,-0.727802722918567,
-2.02351585731242));
#14415=CARTESIAN_POINT('Ctrl Pts',(90.3498698986825,-0.739974677490572,
-2.0176117265465));
#14416=CARTESIAN_POINT('Ctrl Pts',(90.3498698986825,-0.752084605070805,
-2.0115902131628));
#14417=CARTESIAN_POINT('Ctrl Pts',(90.3498698986825,-0.821813208973862,
-1.97691851765953));
#14418=CARTESIAN_POINT('Ctrl Pts',(90.3498698986824,-0.889562996776269,
-1.93832331974276));
#14419=CARTESIAN_POINT('Ctrl Pts',(90.3498698986824,-0.955077779488232,
-1.8960902045986));
#14420=CARTESIAN_POINT('Ctrl Pts',(90.3498698986824,-1.00782120600229,-1.86208995132968));
#14421=CARTESIAN_POINT('Ctrl Pts',(90.3498698986824,-1.05911566374211,-1.82573079164599));
#14422=CARTESIAN_POINT('Ctrl Pts',(90.3498698986824,-1.10880929161885,-1.78714529169388));
#14423=CARTESIAN_POINT('Ctrl Pts',(90.3498698986824,-1.13549274836521,-1.76642644778974));
#14424=CARTESIAN_POINT('Ctrl Pts',(90.3498698986825,-1.16171434281069,-1.74506547534867));
#14425=CARTESIAN_POINT('Ctrl Pts',(90.3498698986825,-1.18744825102446,-1.7230816457625));
#14426=CARTESIAN_POINT('Ctrl Pts',(90.3498698986825,-1.19640383196496,-1.71543111854349));
#14427=CARTESIAN_POINT('Ctrl Pts',(90.3498698986825,-1.20529911666184,-1.70770612424301));
#14428=CARTESIAN_POINT('Ctrl Pts',(90.3498698986825,-1.21412602362739,-1.69991389128877));
#14429=CARTESIAN_POINT('Ctrl Pts',(90.3498698986825,-1.27138360828138,-1.6493679367701));
#14430=CARTESIAN_POINT('Ctrl Pts',(90.3498698986825,-1.32585220395615,-1.59592345890963));
#14431=CARTESIAN_POINT('Ctrl Pts',(90.3498698986825,-1.37729079289597,-1.5398445336051));
#14432=CARTESIAN_POINT('Ctrl Pts',(90.3498698986825,-1.42791166625755,-1.4846570909749));
#14433=CARTESIAN_POINT('Ctrl Pts',(90.3498698986825,-1.47559858119474,-1.4269174071782));
#14434=CARTESIAN_POINT('Ctrl Pts',(90.3498698986825,-1.52007933169395,-1.36685182768371));
#14435=CARTESIAN_POINT('Ctrl Pts',(90.3498698986825,-1.55818476634747,-1.31539529899061));
#14436=CARTESIAN_POINT('Ctrl Pts',(90.3498698986825,-1.59393674881564,-1.26223114492883));
#14437=CARTESIAN_POINT('Ctrl Pts',(90.3498698986825,-1.62713471283201,-1.20749362086063));
#14438=CARTESIAN_POINT('Ctrl Pts',(90.3498698986825,-1.64205050302995,-1.18290014203906));
#14439=CARTESIAN_POINT('Ctrl Pts',(90.3498698986825,-1.65645032490888,-1.15798898503546));
#14440=CARTESIAN_POINT('Ctrl Pts',(90.3498698986825,-1.67031397481906,-1.13277214815257));
#14441=CARTESIAN_POINT('Ctrl Pts',(90.3498698986825,-1.6764049122983,-1.12169323474428));
#14442=CARTESIAN_POINT('Ctrl Pts',(90.3498698986825,-1.68239233832551,-1.11055531714204));
#14443=CARTESIAN_POINT('Ctrl Pts',(90.3498698986825,-1.68827445817782,-1.09935941317281));
#14444=CARTESIAN_POINT('Ctrl Pts',(90.3498698986825,-1.69384736498092,-1.08875205885776));
#14445=CARTESIAN_POINT('Ctrl Pts',(90.3498698986825,-1.69932144666418,-1.07810081173515));
#14446=CARTESIAN_POINT('Ctrl Pts',(90.3498698986825,-1.70469477757152,-1.06740844245853));
#14447=CARTESIAN_POINT('Ctrl Pts',(90.3498698986825,-1.73697093001942,-1.00318225822526));
#14448=CARTESIAN_POINT('Ctrl Pts',(90.3498698986825,-1.76562679488746,-0.937452617252542));
#14449=CARTESIAN_POINT('Ctrl Pts',(90.3498698986825,-1.79041933774232,-0.870427041046266));
#14450=CARTESIAN_POINT('Ctrl Pts',(90.3498698986825,-1.80872633921019,-0.82093484780188));
#14451=CARTESIAN_POINT('Ctrl Pts',(90.3498698986825,-1.82492598563845,-0.770735606083873));
#14452=CARTESIAN_POINT('Ctrl Pts',(90.3498698986825,-1.838902364658,-0.71990970704802));
#14453=CARTESIAN_POINT('Ctrl Pts',(90.3498698986825,-1.8582790431049,-0.649445311297513));
#14454=CARTESIAN_POINT('Ctrl Pts',(90.3498698986825,-1.87338410187543,-0.577775460654213));
#14455=CARTESIAN_POINT('Ctrl Pts',(90.3498698986825,-1.88426075715438,-0.505262831342515));
#14456=CARTESIAN_POINT('Ctrl Pts',(90.3498698986825,-1.8895594387421,-0.469937510832042));
#14457=CARTESIAN_POINT('Ctrl Pts',(90.3498698986825,-1.89385383550029,-0.434412328255347));
#14458=CARTESIAN_POINT('Ctrl Pts',(90.3498698986825,-1.8971447051508,-0.398730679953565));
#14459=CARTESIAN_POINT('Ctrl Pts',(90.3498698986825,-1.89872539720832,-0.381591837015542));
#14460=CARTESIAN_POINT('Ctrl Pts',(90.3498698986825,-1.90007477485771,-0.364410850502331));
#14461=CARTESIAN_POINT('Ctrl Pts',(90.3498698986825,-1.90119093547224,-0.347226454365849));
#14462=CARTESIAN_POINT('Ctrl Pts',(90.3498698986825,-1.90581143780897,-0.276089252899803));
#14463=CARTESIAN_POINT('Ctrl Pts',(90.3498698986825,-1.90645067533891,-0.204804122651826));
#14464=CARTESIAN_POINT('Ctrl Pts',(90.3498698986825,-1.9031984808422,-0.133704998421274));
#14465=CARTESIAN_POINT('Ctrl Pts',(90.3498698986825,-1.89994229664681,-0.0625186518298186));
#14466=CARTESIAN_POINT('Ctrl Pts',(90.3498698986825,-1.8927847725229,0.00848227913307016));
#14467=CARTESIAN_POINT('Ctrl Pts',(90.3498698986825,-1.88176579781181,0.0789493591992786));
#14468=CARTESIAN_POINT('Ctrl Pts',(90.3498698986825,-1.87096201859867,0.148040249667054));
#14469=CARTESIAN_POINT('Ctrl Pts',(90.3498698986825,-1.8564456742516,0.216618795460744));
#14470=CARTESIAN_POINT('Ctrl Pts',(90.3498698986825,-1.83821237884615,0.284329866854858));
#14471=CARTESIAN_POINT('Ctrl Pts',(90.3498698986825,-1.83384319970924,0.30055522787132));
#14472=CARTESIAN_POINT('Ctrl Pts',(90.3498698986825,-1.82926041502798,0.316730622856352));
#14473=CARTESIAN_POINT('Ctrl Pts',(90.3498698986825,-1.82446364132743,0.332850848989154));
#14474=CARTESIAN_POINT('Ctrl Pts',(90.3498698986825,-1.82014892639808,0.34735104947842));
#14475=CARTESIAN_POINT('Ctrl Pts',(90.3498698986825,-1.81565974396159,0.361810316796933));
#14476=CARTESIAN_POINT('Ctrl Pts',(90.3498698986825,-1.81100440526727,0.376199140206947));
#14477=CARTESIAN_POINT('Ctrl Pts',(90.3498698986825,-1.78981976209559,0.441677102094775));
#14478=CARTESIAN_POINT('Ctrl Pts',(90.3498698986825,-1.76516982840305,0.505799597646084));
#14479=CARTESIAN_POINT('Ctrl Pts',(90.3498698986825,-1.73709975902306,0.568253064609059));
#14480=CARTESIAN_POINT('Ctrl Pts',(90.3498698986825,-1.70983211150237,0.628921212611786));
#14481=CARTESIAN_POINT('Ctrl Pts',(90.3498698986825,-1.67933655602438,0.688015070073776));
#14482=CARTESIAN_POINT('Ctrl Pts',(90.3498698986825,-1.64561668449442,0.745217717416419));
#14483=CARTESIAN_POINT('Ctrl Pts',(90.3498698986825,-1.61228551809801,0.801760962404725));
#14484=CARTESIAN_POINT('Ctrl Pts',(90.3498698986825,-1.57580358704956,0.856457003828013));
#14485=CARTESIAN_POINT('Ctrl Pts',(90.3498698986825,-1.5361431033198,0.908960632930662));
#14486=CARTESIAN_POINT('Ctrl Pts',(90.3498698986825,-1.52086991362194,0.929179697644422));
#14487=CARTESIAN_POINT('Ctrl Pts',(90.3498698986825,-1.50512503817007,0.949073159039));
#14488=CARTESIAN_POINT('Ctrl Pts',(90.3498698986825,-1.48890580190333,0.968619417293832));
#14489=CARTESIAN_POINT('',(90.4430005297901,-1.73988535811011,-0.357579366202886));
#14490=CARTESIAN_POINT('Ctrl Pts',(90.3498698986825,-1.48890580190333,0.96861941729381));
#14491=CARTESIAN_POINT('Ctrl Pts',(90.3654557264859,-1.61537991701543,0.774210715156588));
#14492=CARTESIAN_POINT('Ctrl Pts',(90.379221234229,-1.70257359128787,0.556897371306134));
#14493=CARTESIAN_POINT('Ctrl Pts',(90.4021533800625,-1.76705540299077,0.214682455565629));
#14494=CARTESIAN_POINT('Ctrl Pts',(90.4100841123922,-1.77731049373243,0.0986496254663364));
#14495=CARTESIAN_POINT('Ctrl Pts',(90.4263924918293,-1.77503537078494,-0.131797860813206));
#14496=CARTESIAN_POINT('Ctrl Pts',(90.4347211409246,-1.76288391808981,-0.245674537377828));
#14497=CARTESIAN_POINT('Ctrl Pts',(90.4430005297901,-1.73988535811011,-0.357579366202886));
#14498=CARTESIAN_POINT('Ctrl Pts',(90.4431198242969,-1.73921714336317,-0.36081545245689));
#14499=CARTESIAN_POINT('Ctrl Pts',(90.4430800594613,-1.73944088489587,-0.359736964529839));
#14500=CARTESIAN_POINT('Ctrl Pts',(90.4430402946257,-1.73966362327333,-0.358658268489662));
#14501=CARTESIAN_POINT('Ctrl Pts',(90.4430005297901,-1.73988535811011,-0.357579366202887));
#14502=CARTESIAN_POINT('Origin',(88.3562164250559,0.,0.));
#14503=CARTESIAN_POINT('',(90.3498698986825,0.429156946220653,1.72362651929313));
#14504=CARTESIAN_POINT('Origin',(90.3498698986825,0.,0.));
#14505=CARTESIAN_POINT('',(90.4430005297901,-0.906280710947669,1.52765157528285));
#14506=CARTESIAN_POINT('Ctrl Pts',(90.3498698986825,0.429156946220653,1.72362651929313));
#14507=CARTESIAN_POINT('Ctrl Pts',(90.3581493387364,0.318297078944027,1.75122895031072));
#14508=CARTESIAN_POINT('Ctrl Pts',(90.3664780352276,0.205018872177277,1.7680748527967));
#14509=CARTESIAN_POINT('Ctrl Pts',(90.3827864379183,-0.0251386642564886,
1.7798686437189));
#14510=CARTESIAN_POINT('Ctrl Pts',(90.3907171496873,-0.141496109361598,
1.77441601847775));
#14511=CARTESIAN_POINT('Ctrl Pts',(90.4136492336215,-0.486082830458068,
1.72412731573226));
#14512=CARTESIAN_POINT('Ctrl Pts',(90.4274147017556,-0.706812911108985,
1.64598603215369));
#14513=CARTESIAN_POINT('Ctrl Pts',(90.4430005297901,-0.906280710947671,
1.52765157528285));
#14514=CARTESIAN_POINT('Origin',(90.4430005297901,0.,0.));
#14515=CARTESIAN_POINT('Ctrl Pts',(90.1025143645163,1.30770975493414,-1.2010560632029));
#14516=CARTESIAN_POINT('Ctrl Pts',(90.1403023877111,1.68793071858886,-0.787071505416501));
#14517=CARTESIAN_POINT('Ctrl Pts',(90.2158784341009,2.0214346950512,0.423355288987036));
#14518=CARTESIAN_POINT('Ctrl Pts',(90.3292456386917,0.830626863199002,1.8909219215733));
#14519=CARTESIAN_POINT('Ctrl Pts',(90.4048248200878,-0.422610284094226,
1.81385139676035));
#14520=CARTESIAN_POINT('Ctrl Pts',(90.442615978289,-0.906052876477412,1.52699333780199));
#14521=CARTESIAN_POINT('Ctrl Pts',(90.1849662092383,1.41289023394354,-1.29765827295793));
#14522=CARTESIAN_POINT('Ctrl Pts',(90.2227542324332,1.82369277193898,-0.850376499236438));
#14523=CARTESIAN_POINT('Ctrl Pts',(90.2983302788229,2.18402082604052,0.457406202745833));
#14524=CARTESIAN_POINT('Ctrl Pts',(90.4116974834138,0.897435060522396,2.04301077212292));
#14525=CARTESIAN_POINT('Ctrl Pts',(90.4872766648098,-0.45660127632136,1.95974138346671));
#14526=CARTESIAN_POINT('Ctrl Pts',(90.525067823011,-0.978927667841591,1.64981102736054));
#14527=CARTESIAN_POINT('Ctrl Pts',(90.2674180539604,1.51807071295294,-1.39426048271296));
#14528=CARTESIAN_POINT('Ctrl Pts',(90.3052060771553,1.95945482528912,-0.913681493056375));
#14529=CARTESIAN_POINT('Ctrl Pts',(90.3807821235449,2.34660695702982,0.491457116504633));
#14530=CARTESIAN_POINT('Ctrl Pts',(90.4941493281359,0.964243257845793,2.19509962267253));
#14531=CARTESIAN_POINT('Ctrl Pts',(90.5697285095319,-0.490592268548493,
2.10563137017308));
#14532=CARTESIAN_POINT('Ctrl Pts',(90.607519667733,-1.05180245920577,1.77262871691909));
#14533=CARTESIAN_POINT('Ctrl Pts',(90.3498698986825,1.62325119196233,-1.49086269246798));
#14534=CARTESIAN_POINT('Ctrl Pts',(90.3876579218773,2.09521687863925,-0.976986486876311));
#14535=CARTESIAN_POINT('Ctrl Pts',(90.463233968267,2.50919308801913,0.52550803026343));
#14536=CARTESIAN_POINT('Ctrl Pts',(90.5766011728579,1.03105145516918,2.34718847322216));
#14537=CARTESIAN_POINT('Ctrl Pts',(90.6521803542539,-0.524583260775627,
2.25152135687945));
#14538=CARTESIAN_POINT('Ctrl Pts',(90.6899715124551,-1.12467725056995,1.89544640647765));
#14539=CARTESIAN_POINT('',(90.4430005297901,2.20288941995875,0.0846757462792571));
#14540=CARTESIAN_POINT('Ctrl Pts',(90.4430005297901,-0.906280710947677,
1.52765157528285));
#14541=CARTESIAN_POINT('Ctrl Pts',(90.4430005297901,-0.854277760616062,
1.56729260000298));
#14542=CARTESIAN_POINT('Ctrl Pts',(90.4430005297901,-0.800108744344487,
1.60369925011022));
#14543=CARTESIAN_POINT('Ctrl Pts',(90.4430005297901,-0.744125790040279,
1.63692383774151));
#14544=CARTESIAN_POINT('Ctrl Pts',(90.4430005297901,-0.686154010767151,
1.6713287469597));
#14545=CARTESIAN_POINT('Ctrl Pts',(90.4430005297901,-0.626236599116127,
1.70232196503617));
#14546=CARTESIAN_POINT('Ctrl Pts',(90.4430005297901,-0.564718925219456,
1.72992757472046));
#14547=CARTESIAN_POINT('Ctrl Pts',(90.4430005297901,-0.512092172801297,
1.75354344791891));
#14548=CARTESIAN_POINT('Ctrl Pts',(90.4430005297901,-0.458293231174634,
1.77467969048475));
#14549=CARTESIAN_POINT('Ctrl Pts',(90.4430005297901,-0.403518249784151,
1.79332882529259));
#14550=CARTESIAN_POINT('Ctrl Pts',(90.4430005297901,-0.378653325916343,
1.80179453911715));
#14551=CARTESIAN_POINT('Ctrl Pts',(90.4430005297901,-0.353587059186378,
1.80974744290714));
#14552=CARTESIAN_POINT('Ctrl Pts',(90.4430005297901,-0.328336895404217,
1.81718529672686));
#14553=CARTESIAN_POINT('Ctrl Pts',(90.4430005297901,-0.315371182046073,
1.82100456227533));
#14554=CARTESIAN_POINT('Ctrl Pts',(90.4430005297901,-0.302356972411375,
1.82468800737921));
#14555=CARTESIAN_POINT('Ctrl Pts',(90.4430005297901,-0.289296585325211,
1.82823522504611));
#14556=CARTESIAN_POINT('Ctrl Pts',(90.4430005297901,-0.277975229628828,
1.83131011958596));
#14557=CARTESIAN_POINT('Ctrl Pts',(90.4430005297901,-0.266619082046204,
1.83428258023668));
#14558=CARTESIAN_POINT('Ctrl Pts',(90.4430005297901,-0.255244023393878,
1.83714894810172));
#14559=CARTESIAN_POINT('Ctrl Pts',(90.4430005297901,-0.186918851849708,
1.85436600887245));
#14560=CARTESIAN_POINT('Ctrl Pts',(90.4430005297901,-0.117787865443795,
1.8677937815248));
#14561=CARTESIAN_POINT('Ctrl Pts',(90.4430005297901,-0.0482176105662551,
1.87746078885698));
#14562=CARTESIAN_POINT('Ctrl Pts',(90.4430005297901,0.0225458393465897,
1.88729359441967));
#14563=CARTESIAN_POINT('Ctrl Pts',(90.4430005297901,0.0937646734743491,
1.89323595416038));
#14564=CARTESIAN_POINT('Ctrl Pts',(90.4430005297901,0.165083212114906,1.89527294746021));
#14565=CARTESIAN_POINT('Ctrl Pts',(90.4430005297901,0.235975923373851,1.89729777831897));
#14566=CARTESIAN_POINT('Ctrl Pts',(90.4430005297901,0.306968202656807,1.89546400374334));
#14567=CARTESIAN_POINT('Ctrl Pts',(90.4430005297901,0.377725173679162,1.88970801775622));
#14568=CARTESIAN_POINT('Ctrl Pts',(90.4430005297901,0.38708606610097,1.88894652154138));
#14569=CARTESIAN_POINT('Ctrl Pts',(90.4430005297901,0.396442847540757,1.88811630351685));
#14570=CARTESIAN_POINT('Ctrl Pts',(90.4430005297901,0.405794746349182,1.88721714781831));
#14571=CARTESIAN_POINT('Ctrl Pts',(90.4430005297901,0.41906845278398,1.88594092263387));
#14572=CARTESIAN_POINT('Ctrl Pts',(90.4430005297901,0.432332323108797,1.88452581977721));
#14573=CARTESIAN_POINT('Ctrl Pts',(90.4430005297901,0.4455841469567,1.88297116443225));
#14574=CARTESIAN_POINT('Ctrl Pts',(90.4430005297901,0.458728559964043,1.88142911013294));
#14575=CARTESIAN_POINT('Ctrl Pts',(90.4430005297901,0.471853391141752,1.87975060439521));
#14576=CARTESIAN_POINT('Ctrl Pts',(90.4430005297901,0.484948310227801,1.8779367216178));
#14577=CARTESIAN_POINT('Ctrl Pts',(90.4430005297901,0.557788263474281,1.86784707266058));
#14578=CARTESIAN_POINT('Ctrl Pts',(90.4430005297901,0.629779464650553,1.85356363281223));
#14579=CARTESIAN_POINT('Ctrl Pts',(90.4430005297901,0.700551912386958,1.83508091077558));
#14580=CARTESIAN_POINT('Ctrl Pts',(90.4430005297901,0.732380673074804,1.82676860626471));
#14581=CARTESIAN_POINT('Ctrl Pts',(90.4430005297901,0.763963163282864,1.81760628974152));
#14582=CARTESIAN_POINT('Ctrl Pts',(90.4430005297901,0.795266463078768,1.80759010215849));
#14583=CARTESIAN_POINT('Ctrl Pts',(90.4430005297901,0.863383166190852,1.78579464671587));
#14584=CARTESIAN_POINT('Ctrl Pts',(90.4430005297901,0.930178515592966,1.75995975736864));
#14585=CARTESIAN_POINT('Ctrl Pts',(90.4430005297901,0.995462794522614,1.73037590133247));
#14586=CARTESIAN_POINT('Ctrl Pts',(90.4430005297901,1.05348264614204,1.70408395224931));
#14587=CARTESIAN_POINT('Ctrl Pts',(90.4430005297901,1.11030929879789,1.67482990061158));
#14588=CARTESIAN_POINT('Ctrl Pts',(90.4430005297901,1.16580106122498,1.64278422184805));
#14589=CARTESIAN_POINT('Ctrl Pts',(90.4430005297901,1.1762422869831,1.63675456714062));
#14590=CARTESIAN_POINT('Ctrl Pts',(90.4430005297901,1.18662850495694,1.63063043366675));
#14591=CARTESIAN_POINT('Ctrl Pts',(90.4430005297901,1.19695660054926,1.62441474165913));
#14592=CARTESIAN_POINT('Ctrl Pts',(90.4430005297901,1.25999165646837,1.58647875532222));
#14593=CARTESIAN_POINT('Ctrl Pts',(90.4430005297901,1.32088999310675,1.54512054405464));
#14594=CARTESIAN_POINT('Ctrl Pts',(90.4430005297901,1.37946364276531,1.50067032140515));
#14595=CARTESIAN_POINT('Ctrl Pts',(90.4430005297901,1.43980234042177,1.45488064360901));
#14596=CARTESIAN_POINT('Ctrl Pts',(90.4430005297901,1.4976749624294,1.40580945467811));
#14597=CARTESIAN_POINT('Ctrl Pts',(90.4430005297901,1.55286316603457,1.35376300243271));
#14598=CARTESIAN_POINT('Ctrl Pts',(90.4430005297901,1.60805136963973,1.30171655018731));
#14599=CARTESIAN_POINT('Ctrl Pts',(90.4430005297901,1.66055597517919,1.2466941849305));
#14600=CARTESIAN_POINT('Ctrl Pts',(90.4430005297901,1.71013357145278,1.18895618401778));
#14601=CARTESIAN_POINT('Ctrl Pts',(90.4430005297901,1.72296507476095,1.17401263278891));
#14602=CARTESIAN_POINT('Ctrl Pts',(90.4430005297901,1.73560034241773,1.15888696127208));
#14603=CARTESIAN_POINT('Ctrl Pts',(90.4430005297901,1.74803477487696,1.14358326375263));
#14604=CARTESIAN_POINT('Ctrl Pts',(90.4430005297901,1.76083174777711,1.12783336900912));
#14605=CARTESIAN_POINT('Ctrl Pts',(90.4430005297901,1.77341879728594,1.11189092493475));
#14606=CARTESIAN_POINT('Ctrl Pts',(90.4430005297901,1.78576841317893,1.09579034652113));
#14607=CARTESIAN_POINT('Ctrl Pts',(90.4430005297901,1.83344349969788,1.03363485314175));
#14608=CARTESIAN_POINT('Ctrl Pts',(90.4430005297901,1.87765235974256,0.96904318706518));
#14609=CARTESIAN_POINT('Ctrl Pts',(90.4430005297901,1.91815905620923,0.902327591860497));
#14610=CARTESIAN_POINT('Ctrl Pts',(90.4430005297901,1.95747515213314,0.837572947086005));
#14611=CARTESIAN_POINT('Ctrl Pts',(90.4430005297901,1.99330413338327,0.770816566121482));
#14612=CARTESIAN_POINT('Ctrl Pts',(90.4430005297901,2.02539955299598,0.702308430193654));
#14613=CARTESIAN_POINT('Ctrl Pts',(90.4430005297901,2.03357309269832,0.684861891849646));
#14614=CARTESIAN_POINT('Ctrl Pts',(90.4430005297901,2.04150431230281,0.667301596050367));
#14615=CARTESIAN_POINT('Ctrl Pts',(90.4430005297901,2.04918873720806,0.649631385046051));
#14616=CARTESIAN_POINT('Ctrl Pts',(90.4430005297901,2.05671130248248,0.632333367649584));
#14617=CARTESIAN_POINT('Ctrl Pts',(90.4430005297901,2.06399514527129,0.614934728437702));
#14618=CARTESIAN_POINT('Ctrl Pts',(90.4430005297901,2.07103059613546,0.597454518134323));
#14619=CARTESIAN_POINT('Ctrl Pts',(90.4430005297901,2.09104535379643,0.547726052988361));
#14620=CARTESIAN_POINT('Ctrl Pts',(90.4430005297901,2.10906573010327,0.497303151678278));
#14621=CARTESIAN_POINT('Ctrl Pts',(90.4430005297901,2.12501355371715,0.446278571766078));
#14622=CARTESIAN_POINT('Ctrl Pts',(90.4430005297901,2.14793295022753,0.372948654963803));
#14623=CARTESIAN_POINT('Ctrl Pts',(90.4430005297901,2.16657429828593,0.298376904723251));
#14624=CARTESIAN_POINT('Ctrl Pts',(90.4430005297901,2.18107268216625,0.222889057559564));
#14625=CARTESIAN_POINT('Ctrl Pts',(90.4430005297901,2.18985901387143,0.177141802529971));
#14626=CARTESIAN_POINT('Ctrl Pts',(90.4430005297901,2.19712286143422,0.131057562795162));
#14627=CARTESIAN_POINT('Ctrl Pts',(90.4430005297901,2.2028857444688,0.0847053108012291));
#14628=CARTESIAN_POINT('',(90.3497506833166,0.432411172325593,1.72302747110366));
#14629=CARTESIAN_POINT('Ctrl Pts',(90.3498698986825,0.429156946220652,1.72362651929313));
#14630=CARTESIAN_POINT('Ctrl Pts',(90.3498301602272,0.430225058085747,1.72336057558601));
#14631=CARTESIAN_POINT('Ctrl Pts',(90.3497904217719,0.431292922747308,1.72309363903332));
#14632=CARTESIAN_POINT('Ctrl Pts',(90.3497506833166,0.432360538359997,1.72282571009637));
#14633=CARTESIAN_POINT('',(90.3498698986825,1.62325119196235,-1.49086269246796));
#14634=CARTESIAN_POINT('Ctrl Pts',(90.3498698986825,0.432473260079399,1.72322635770742));
#14635=CARTESIAN_POINT('Ctrl Pts',(90.3498698986825,0.500689037073848,1.71492876273114));
#14636=CARTESIAN_POINT('Ctrl Pts',(90.3498698986825,0.568201159921544,1.7026236132268));
#14637=CARTESIAN_POINT('Ctrl Pts',(90.3498698986825,0.63464679981471,1.68629351059737));
#14638=CARTESIAN_POINT('Ctrl Pts',(90.3498698986825,0.66677182170839,1.67839826110711));
#14639=CARTESIAN_POINT('Ctrl Pts',(90.3498698986825,0.698647807968663,1.66956143909895));
#14640=CARTESIAN_POINT('Ctrl Pts',(90.3498698986825,0.730234584403305,1.65977677709578));
#14641=CARTESIAN_POINT('Ctrl Pts',(90.3498698986825,0.781946426308745,1.64375795682607));
#14642=CARTESIAN_POINT('Ctrl Pts',(90.3498698986825,0.832883402990908,1.62519998965726));
#14643=CARTESIAN_POINT('Ctrl Pts',(90.3498698986825,0.88294589212397,1.60424660726948));
#14644=CARTESIAN_POINT('Ctrl Pts',(90.3498698986825,0.894457590187191,1.5994284486915));
#14645=CARTESIAN_POINT('Ctrl Pts',(90.3498698986825,0.905920948354246,1.59448434130905));
#14646=CARTESIAN_POINT('Ctrl Pts',(90.3498698986825,0.917326683635254,1.58941980305414));
#14647=CARTESIAN_POINT('Ctrl Pts',(90.3498698986825,0.979664976023323,1.56173945989633));
#14648=CARTESIAN_POINT('Ctrl Pts',(90.3498698986825,1.0403517211105,1.53043727360066));
#14649=CARTESIAN_POINT('Ctrl Pts',(90.3498698986825,1.09919843952219,1.49582959807598));
#14650=CARTESIAN_POINT('Ctrl Pts',(90.3498698986825,1.15010544628058,1.46589125623842));
#14651=CARTESIAN_POINT('Ctrl Pts',(90.3498698986825,1.19963574840112,1.43347809869087));
#14652=CARTESIAN_POINT('Ctrl Pts',(90.3498698986825,1.24766201189904,1.39876400501927));
#14653=CARTESIAN_POINT('Ctrl Pts',(90.3498698986825,1.26296034952528,1.38770614028658));
#14654=CARTESIAN_POINT('Ctrl Pts',(90.3498698986825,1.27810601388692,1.37641460218754));
#14655=CARTESIAN_POINT('Ctrl Pts',(90.3498698986825,1.29309468960961,1.36489446808101));
#14656=CARTESIAN_POINT('Ctrl Pts',(90.3498698986825,1.30640467453454,1.35466455757203));
#14657=CARTESIAN_POINT('Ctrl Pts',(90.3498698986825,1.31959368966207,1.34425192002828));
#14658=CARTESIAN_POINT('Ctrl Pts',(90.3498698986825,1.33263794396078,1.33367724437743));
#14659=CARTESIAN_POINT('Ctrl Pts',(90.3498698986825,1.38778035157091,1.28897456826191));
#14660=CARTESIAN_POINT('Ctrl Pts',(90.3498698986825,1.44040951217242,1.24132658210685));
#14661=CARTESIAN_POINT('Ctrl Pts',(90.3498698986825,1.49033018861726,1.19105566689337));
#14662=CARTESIAN_POINT('Ctrl Pts',(90.3498698986825,1.54132495686097,1.13970312415401));
#14663=CARTESIAN_POINT('Ctrl Pts',(90.3498698986825,1.58949432651507,1.08561309730986));
#14664=CARTESIAN_POINT('Ctrl Pts',(90.3498698986825,1.63461237105893,1.02907775276922));
#14665=CARTESIAN_POINT('Ctrl Pts',(90.3498698986825,1.67109719589425,0.983360298402049));
#14666=CARTESIAN_POINT('Ctrl Pts',(90.3498698986825,1.70558655725381,0.936042670410925));
#14667=CARTESIAN_POINT('Ctrl Pts',(90.3498698986825,1.73794656373637,0.887259053299169));
#14668=CARTESIAN_POINT('Ctrl Pts',(90.3498698986825,1.75291021222756,0.864700933634309));
#14669=CARTESIAN_POINT('Ctrl Pts',(90.3498698986825,1.76741833878176,0.841829120502184));
#14670=CARTESIAN_POINT('Ctrl Pts',(90.3498698986825,1.78145646826647,0.818655805601394));
#14671=CARTESIAN_POINT('Ctrl Pts',(90.3498698986825,1.7878902939984,0.808035226138498));
#14672=CARTESIAN_POINT('Ctrl Pts',(90.3498698986825,1.79422637477591,0.797349598647965));
#14673=CARTESIAN_POINT('Ctrl Pts',(90.3498698986825,1.8004601115605,0.786605484523137));
#14674=CARTESIAN_POINT('Ctrl Pts',(90.3498698986825,1.83793113462181,0.722022560659537));
#14675=CARTESIAN_POINT('Ctrl Pts',(90.3498698986825,1.87157440109755,0.655560357407762));
#14676=CARTESIAN_POINT('Ctrl Pts',(90.3498698986825,1.9011666568507,0.587535602339381));
#14677=CARTESIAN_POINT('Ctrl Pts',(90.3498698986825,1.92600732300679,0.530433492750316));
#14678=CARTESIAN_POINT('Ctrl Pts',(90.3498698986825,1.94799336759623,0.47222923559375));
#14679=CARTESIAN_POINT('Ctrl Pts',(90.3498698986825,1.96697450572884,0.41308845846253));
#14680=CARTESIAN_POINT('Ctrl Pts',(90.3498698986825,1.98906817163189,0.344249774393362));
#14681=CARTESIAN_POINT('Ctrl Pts',(90.3498698986825,2.007092396991,0.274142320643778));
#14682=CARTESIAN_POINT('Ctrl Pts',(90.3498698986825,2.02116104200529,0.20307430952008));
#14683=CARTESIAN_POINT('Ctrl Pts',(90.3498698986825,2.02849211048846,0.166041286369528));
#14684=CARTESIAN_POINT('Ctrl Pts',(90.3498698986825,2.03474828995461,0.128747041232483));
#14685=CARTESIAN_POINT('Ctrl Pts',(90.3498698986825,2.03994046639292,0.0912332730845031));
#14686=CARTESIAN_POINT('Ctrl Pts',(90.3498698986825,2.04159548143424,0.0792756958951641));
#14687=CARTESIAN_POINT('Ctrl Pts',(90.3498698986825,2.04314268181887,0.0672931065835388));
#14688=CARTESIAN_POINT('Ctrl Pts',(90.3498698986825,2.04458127608794,0.0552958865448525));
#14689=CARTESIAN_POINT('Ctrl Pts',(90.3498698986825,2.05337295176474,-0.0180226785786454));
#14690=CARTESIAN_POINT('Ctrl Pts',(90.3498698986825,2.05809534086541,-0.0917277015695579));
#14691=CARTESIAN_POINT('Ctrl Pts',(90.3498698986825,2.05891131036709,-0.165484762976481));
#14692=CARTESIAN_POINT('Ctrl Pts',(90.3498698986825,2.05975504538853,-0.241751603415596));
#14693=CARTESIAN_POINT('Ctrl Pts',(90.3498698986825,2.05642222258581,-0.31807488200744));
#14694=CARTESIAN_POINT('Ctrl Pts',(90.3498698986825,2.04904110315226,-0.394108580280238));
#14695=CARTESIAN_POINT('Ctrl Pts',(90.3498698986825,2.04165998371871,-0.47014227855304));
#14696=CARTESIAN_POINT('Ctrl Pts',(90.3498698986825,2.03023052285033,-0.545887393002507));
#14697=CARTESIAN_POINT('Ctrl Pts',(90.3498698986825,2.01482901135003,-0.621007387284477));
#14698=CARTESIAN_POINT('Ctrl Pts',(90.3498698986825,2.0082558082846,-0.653067810489036));
#14699=CARTESIAN_POINT('Ctrl Pts',(90.3498698986825,2.00095845789534,-0.685014398435953));
#14700=CARTESIAN_POINT('Ctrl Pts',(90.3498698986825,1.99294003791299,-0.716820819516162));
#14701=CARTESIAN_POINT('Ctrl Pts',(90.3498698986825,1.98892248395689,-0.732757127806477));
#14702=CARTESIAN_POINT('Ctrl Pts',(90.3498698986825,1.98472264433957,-0.748662300766758));
#14703=CARTESIAN_POINT('Ctrl Pts',(90.3498698986825,1.98034860459119,-0.764505835419566));
#14704=CARTESIAN_POINT('Ctrl Pts',(90.3498698986825,1.95934426572443,-0.840587213239224));
#14705=CARTESIAN_POINT('Ctrl Pts',(90.3498698986825,1.93430052129815,-0.91536072687171));
#14706=CARTESIAN_POINT('Ctrl Pts',(90.3498698986825,1.90535385031768,-0.988470818953257));
#14707=CARTESIAN_POINT('Ctrl Pts',(90.3498698986825,1.87638204882009,-1.06164438273494));
#14708=CARTESIAN_POINT('Ctrl Pts',(90.3498698986825,1.8435004604687,-1.13315267365607));
#14709=CARTESIAN_POINT('Ctrl Pts',(90.3498698986825,1.80679432959692,-1.20264141611964));
#14710=CARTESIAN_POINT('Ctrl Pts',(90.3498698986825,1.7704793662928,-1.27138963535931));
#14711=CARTESIAN_POINT('Ctrl Pts',(90.3498698986825,1.73042077500635,-1.33816212418963));
#14712=CARTESIAN_POINT('Ctrl Pts',(90.3498698986825,1.68665261190661,-1.4026027958059));
#14713=CARTESIAN_POINT('Ctrl Pts',(90.3498698986825,1.66632005262628,-1.43253879683743));
#14714=CARTESIAN_POINT('Ctrl Pts',(90.3498698986825,1.64518626524376,-1.46197129625266));
#14715=CARTESIAN_POINT('Ctrl Pts',(90.3498698986825,1.62325119196239,-1.49086269246791));
#14716=CARTESIAN_POINT('Ctrl Pts',(90.3498698986825,1.62325119196235,-1.49086269246796));
#14717=CARTESIAN_POINT('Ctrl Pts',(90.380913442385,2.01097952971941,-1.06870410630073));
#14718=CARTESIAN_POINT('Ctrl Pts',(90.4119569860876,2.21987663538069,-0.486345711720857));
#14719=CARTESIAN_POINT('Ctrl Pts',(90.4430005297901,2.20288941995875,0.0846757462792571));
#14720=CARTESIAN_POINT('Origin',(90.3498698986825,-2.40291074888303E-16,
0.));
#14721=CARTESIAN_POINT('',(90.3498698986825,-2.69912154532077E-16,2.204));
#14722=CARTESIAN_POINT('Origin',(90.3498698986825,0.,0.));
#14723=CARTESIAN_POINT('Origin',(90.3498698986825,0.,0.));
#14724=CARTESIAN_POINT('Origin',(66.9212607628943,0.,0.));
#14725=CARTESIAN_POINT('',(81.4430005297901,-2.69912154532077E-16,2.204));
#14726=CARTESIAN_POINT('Origin',(81.4430005297901,0.,0.));
#14727=CARTESIAN_POINT('',(66.9212607628943,-2.69912154532077E-16,2.204));
#14728=CARTESIAN_POINT('Origin',(90.4430005297901,0.,0.));
#14729=CARTESIAN_POINT('Ctrl Pts',(82.0295201802136,-1.65306427348725,3.32899555241991));
#14730=CARTESIAN_POINT('Ctrl Pts',(82.0621173237355,-2.19852390520666,3.05813912872495));
#14731=CARTESIAN_POINT('Ctrl Pts',(82.1273116107797,-3.14747075323877,2.24346380767911));
#14732=CARTESIAN_POINT('Ctrl Pts',(82.257700184868,-4.08359169347408,-0.09571649437622));
#14733=CARTESIAN_POINT('Ctrl Pts',(82.4206859024783,-2.86883663152734,-3.29923455674864));
#14734=CARTESIAN_POINT('Ctrl Pts',(82.6162687636106,1.16238339903618,-4.2168753806827));
#14735=CARTESIAN_POINT('Ctrl Pts',(82.811851624743,4.15031934985653,-1.37057296918483));
#14736=CARTESIAN_POINT('Ctrl Pts',(83.0074344858754,3.44345504116371,2.69406016453184));
#14737=CARTESIAN_POINT('Ctrl Pts',(83.2030173470079,-0.333719683741995,
4.35943641705783));
#14738=CARTESIAN_POINT('Ctrl Pts',(83.39860020814,-3.81263960805445,2.13930714802621));
#14739=CARTESIAN_POINT('Ctrl Pts',(83.5941830692725,-3.8944646466128,-1.98684861864105));
#14740=CARTESIAN_POINT('Ctrl Pts',(83.7897659304049,-0.50564373165627,-4.3426562533637));
#14741=CARTESIAN_POINT('Ctrl Pts',(83.9853487915373,3.3336643879048,-2.8285491238196));
#14742=CARTESIAN_POINT('Ctrl Pts',(84.1809316526696,4.20232603899528,1.20609443396036));
#14743=CARTESIAN_POINT('Ctrl Pts',(84.3765145138021,1.32618441591987,4.16598292634243));
#14744=CARTESIAN_POINT('Ctrl Pts',(84.5720973749343,-2.73173526363988,3.41346879580696));
#14745=CARTESIAN_POINT('Ctrl Pts',(84.7676802360668,-4.35535562891122,-0.380852351780076));
#14746=CARTESIAN_POINT('Ctrl Pts',(84.963263097199,-2.09782657360965,-3.83579056771449));
#14747=CARTESIAN_POINT('Ctrl Pts',(85.1588459583315,2.02911726294498,-3.87257613345951));
#14748=CARTESIAN_POINT('Ctrl Pts',(85.3544288194639,4.34787387083917,-0.458430425156126));
#14749=CARTESIAN_POINT('Ctrl Pts',(85.5500116805963,2.7921507497253,3.36423229852469));
#14750=CARTESIAN_POINT('Ctrl Pts',(85.7455945417287,-1.25171488096045,4.18895863102669));
#14751=CARTESIAN_POINT('Ctrl Pts',(85.9411774028608,-4.18015184799219,1.28081826434192));
#14752=CARTESIAN_POINT('Ctrl Pts',(86.1367602639934,-3.38356990681389,-2.76868550442667));
#14753=CARTESIAN_POINT('Ctrl Pts',(86.3323431251257,0.428180394291547,-4.35095693918743));
#14754=CARTESIAN_POINT('Ctrl Pts',(86.5279259862581,3.85837041772825,-2.05600160947017));
#14755=CARTESIAN_POINT('Ctrl Pts',(86.7235088473905,3.85028754068497,2.07109884112684));
#14756=CARTESIAN_POINT('Ctrl Pts',(86.9190917085228,0.4111347439794,4.3526007156551));
#14757=CARTESIAN_POINT('Ctrl Pts',(87.1146745696552,-3.39438885318226,2.7554110337347));
#14758=CARTESIAN_POINT('Ctrl Pts',(87.3102574307876,-4.17510263508425,-1.29718185414927));
#14759=CARTESIAN_POINT('Ctrl Pts',(87.50584029192,-1.23529790690718,-4.19382935913003));
#14760=CARTESIAN_POINT('Ctrl Pts',(87.7014231530522,2.80530789506251,-3.35326986418407));
#14761=CARTESIAN_POINT('Ctrl Pts',(87.8970060141848,4.34604268780248,0.475457386481673));
#14762=CARTESIAN_POINT('Ctrl Pts',(88.092588875317,2.01393751246173,3.88049411074219));
#14763=CARTESIAN_POINT('Ctrl Pts',(88.2881717364494,-2.11284414771308,3.82754458225146));
#14764=CARTESIAN_POINT('Ctrl Pts',(88.4837545975819,-4.35679539852597,0.36378874697873));
#14765=CARTESIAN_POINT('Ctrl Pts',(88.6793374587141,-2.71838192148609,-3.42414057059281));
#14766=CARTESIAN_POINT('Ctrl Pts',(88.8749203198466,1.34256965287038,-4.16076063290167));
#14767=CARTESIAN_POINT('Ctrl Pts',(89.0705031809788,4.20685975871864,-1.18961625113958));
#14768=CARTESIAN_POINT('Ctrl Pts',(89.2660860421113,3.322882630607,2.84156747674539));
#14769=CARTESIAN_POINT('Ctrl Pts',(89.4616689032436,-0.523309385250935,
4.34067852736659));
#14770=CARTESIAN_POINT('Ctrl Pts',(89.6572517643761,-3.9008702141681,1.97150514629555));
#14771=CARTESIAN_POINT('Ctrl Pts',(89.8528346255084,-3.80698675149828,-2.15407172965046));
#14772=CARTESIAN_POINT('Ctrl Pts',(90.0484174866407,-0.310961962579554,
-4.3610176492037));
#14773=CARTESIAN_POINT('Ctrl Pts',(90.211403204251,2.81536141761182,-2.95949706107794));
#14774=CARTESIAN_POINT('Ctrl Pts',(90.3418371019651,3.81133709361766,-0.644214494217));
#14775=CARTESIAN_POINT('Ctrl Pts',(90.4070767126353,3.71781142410833,0.603927146986502));
#14776=CARTESIAN_POINT('Ctrl Pts',(90.4397191797832,3.52383717212292,1.18211855844504));
#14777=CARTESIAN_POINT('Ctrl Pts',(82.1685848090598,-1.76019011105466,3.54472911011085));
#14778=CARTESIAN_POINT('Ctrl Pts',(82.2011819525819,-2.34099792665557,3.25631999852939));
#14779=CARTESIAN_POINT('Ctrl Pts',(82.2663762396261,-3.35144070532561,2.38885013252105));
#14780=CARTESIAN_POINT('Ctrl Pts',(82.3967648137143,-4.34822640094612,-0.101919344315883));
#14781=CARTESIAN_POINT('Ctrl Pts',(82.5597505313248,-3.05474986667829,-3.51303947098677));
#14782=CARTESIAN_POINT('Ctrl Pts',(82.7553333924568,1.23771095719187,-4.49014745746654));
#14783=CARTESIAN_POINT('Ctrl Pts',(82.9509162535894,4.41927830303003,-1.45939212741482));
#14784=CARTESIAN_POINT('Ctrl Pts',(83.1464991147216,3.66660607728902,2.86864711569356));
#14785=CARTESIAN_POINT('Ctrl Pts',(83.3420819758541,-0.355346187446032,
4.64194707619514));
#14786=CARTESIAN_POINT('Ctrl Pts',(83.5376648369865,-4.05971542833935,2.2779436630861));
#14787=CARTESIAN_POINT('Ctrl Pts',(83.7332476981189,-4.146843089385,-2.11560515025648));
#14788=CARTESIAN_POINT('Ctrl Pts',(83.9288305592512,-0.538411670043889,
-4.6240794840694));
#14789=CARTESIAN_POINT('Ctrl Pts',(84.1244134203835,3.54970050667567,-3.01185155122646));
#14790=CARTESIAN_POINT('Ctrl Pts',(84.319996281516,4.47465525442806,1.28425465948555));
#14791=CARTESIAN_POINT('Ctrl Pts',(84.5155791426482,1.41212700061114,4.435956948184));
#14792=CARTESIAN_POINT('Ctrl Pts',(84.7111620037808,-2.90876372697514,3.63467659130886));
#14793=CARTESIAN_POINT('Ctrl Pts',(84.9067448649131,-4.63760183502324,-0.405533259732842));
#14794=CARTESIAN_POINT('Ctrl Pts',(85.1023277260453,-2.23377496495383,-4.08436667203786));
#14795=CARTESIAN_POINT('Ctrl Pts',(85.2979105871779,2.16061298867192,-4.12353610428102));
#14796=CARTESIAN_POINT('Ctrl Pts',(85.4934934483101,4.62963522611218,-0.488138733567902));
#14797=CARTESIAN_POINT('Ctrl Pts',(85.6890763094425,2.97309440235643,3.58224935238705));
#14798=CARTESIAN_POINT('Ctrl Pts',(85.884659170575,-1.33283151215811,4.46042157961329));
#14799=CARTESIAN_POINT('Ctrl Pts',(86.0802420317073,-4.45104407829276,1.36382092282285));
#14800=CARTESIAN_POINT('Ctrl Pts',(86.2758248928396,-3.60284012276907,-2.94810850592725));
#14801=CARTESIAN_POINT('Ctrl Pts',(86.471407753972,0.455928367618472,-4.63291809085333));
#14802=CARTESIAN_POINT('Ctrl Pts',(86.6669906151044,4.10840979567241,-2.18923955912946));
#14803=CARTESIAN_POINT('Ctrl Pts',(86.8625734762367,4.09980311263617,2.20531515781764));
#14804=CARTESIAN_POINT('Ctrl Pts',(87.0581563373692,0.437778084173888,4.63466839126788));
#14805=CARTESIAN_POINT('Ctrl Pts',(87.2537391985015,-3.61436018445999,2.93397379113351));
#14806=CARTESIAN_POINT('Ctrl Pts',(87.4493220596338,-4.44566765417441,-1.38124494524121));
#14807=CARTESIAN_POINT('Ctrl Pts',(87.6449049207663,-1.31535064595982,-4.46560795232644));
#14808=CARTESIAN_POINT('Ctrl Pts',(87.8404877818986,2.98710418859627,-3.57057650407201));
#14809=CARTESIAN_POINT('Ctrl Pts',(88.036070643031,4.62768537435842,0.506269116897338));
#14810=CARTESIAN_POINT('Ctrl Pts',(88.2316535041634,2.14444952357415,4.13196720132669));
#14811=CARTESIAN_POINT('Ctrl Pts',(88.4272363652956,-2.24976574392887,4.07558631043868));
#14812=CARTESIAN_POINT('Ctrl Pts',(88.6228192264281,-4.63913490804326,0.387363858269165));
#14813=CARTESIAN_POINT('Ctrl Pts',(88.8184020875603,-2.89454502950186,-3.64603994405123));
#14814=CARTESIAN_POINT('Ctrl Pts',(89.013984948693,1.42957407300277,-4.43039622715286));
#14815=CARTESIAN_POINT('Ctrl Pts',(89.2095678098251,4.47948277913555,-1.26670861792234));
#14816=CARTESIAN_POINT('Ctrl Pts',(89.4051506709576,3.5382200440707,3.02571355069598));
#14817=CARTESIAN_POINT('Ctrl Pts',(89.60073353209,-0.557222135711404,4.62197359272669));
#14818=CARTESIAN_POINT('Ctrl Pts',(89.7963163932224,-4.15366376589914,2.09926735339947));
#14819=CARTESIAN_POINT('Ctrl Pts',(89.9918992543546,-4.05369624180864,-2.29366505455626));
#14820=CARTESIAN_POINT('Ctrl Pts',(90.1874821154872,-0.331113665829834,
-4.64363077914069));
#14821=CARTESIAN_POINT('Ctrl Pts',(90.3504678330974,2.99780922363717,-3.15128549092374));
#14822=CARTESIAN_POINT('Ctrl Pts',(90.4809017308115,4.05832850523665,-0.685962427659713));
#14823=CARTESIAN_POINT('Ctrl Pts',(90.5461413414815,3.95874196087756,0.643064283084749));
#14824=CARTESIAN_POINT('Ctrl Pts',(90.5787838086296,3.75219732397504,1.25872504175513));
#14825=CARTESIAN_POINT('Ctrl Pts',(82.3076494379063,-1.86731594862207,3.76046266780178));
#14826=CARTESIAN_POINT('Ctrl Pts',(82.3402465814283,-2.48347194810449,3.45450086833384));
#14827=CARTESIAN_POINT('Ctrl Pts',(82.4054408684725,-3.55541065741244,2.53423645736299));
#14828=CARTESIAN_POINT('Ctrl Pts',(82.5358294425606,-4.61286110841813,-0.108122194255548));
#14829=CARTESIAN_POINT('Ctrl Pts',(82.698815160171,-3.24066310182923,-3.7268443852249));
#14830=CARTESIAN_POINT('Ctrl Pts',(82.8943980213033,1.31303851534757,-4.76341953425041));
#14831=CARTESIAN_POINT('Ctrl Pts',(83.0899808824357,4.68823725620352,-1.5482112856448));
#14832=CARTESIAN_POINT('Ctrl Pts',(83.2855637435681,3.88975711341433,3.04323406685525));
#14833=CARTESIAN_POINT('Ctrl Pts',(83.4811466047003,-0.376972691150075,
4.92445773533245));
#14834=CARTESIAN_POINT('Ctrl Pts',(83.6767294658329,-4.30679124862426,2.41658017814598));
#14835=CARTESIAN_POINT('Ctrl Pts',(83.8723123269652,-4.39922153215723,-2.2443616818719));
#14836=CARTESIAN_POINT('Ctrl Pts',(84.0678951880976,-0.571179608431502,
-4.90550271477511));
#14837=CARTESIAN_POINT('Ctrl Pts',(84.26347804923,3.76573662544653,-3.19515397863332));
#14838=CARTESIAN_POINT('Ctrl Pts',(84.4590609103622,4.74698446986084,1.36241488501073));
#14839=CARTESIAN_POINT('Ctrl Pts',(84.6546437714947,1.4980695853024,4.70593097002559));
#14840=CARTESIAN_POINT('Ctrl Pts',(84.850226632627,-3.08579219031039,3.85588438681077));
#14841=CARTESIAN_POINT('Ctrl Pts',(85.0458094937594,-4.91984804113526,-0.430214167685617));
#14842=CARTESIAN_POINT('Ctrl Pts',(85.2413923548919,-2.369723356298,-4.33294277636122));
#14843=CARTESIAN_POINT('Ctrl Pts',(85.4369752160242,2.29210871439886,-4.37449607510255));
#14844=CARTESIAN_POINT('Ctrl Pts',(85.6325580771566,4.91139658138516,-0.517847041979676));
#14845=CARTESIAN_POINT('Ctrl Pts',(85.8281409382889,3.15403805498757,3.80026640624941));
#14846=CARTESIAN_POINT('Ctrl Pts',(86.0237237994213,-1.41394814335575,4.73188452819988));
#14847=CARTESIAN_POINT('Ctrl Pts',(86.2193066605536,-4.72193630859334,1.44682358130377));
#14848=CARTESIAN_POINT('Ctrl Pts',(86.414889521686,-3.82211033872426,-3.12753150742783));
#14849=CARTESIAN_POINT('Ctrl Pts',(86.6104723828184,0.483676340945399,-4.91487924251923));
#14850=CARTESIAN_POINT('Ctrl Pts',(86.8060552439507,4.35844917361658,-2.32247750878875));
#14851=CARTESIAN_POINT('Ctrl Pts',(87.0016381050832,4.34931868458738,2.33953147450845));
#14852=CARTESIAN_POINT('Ctrl Pts',(87.1972209662155,0.464421424368368,4.91673606688068));
#14853=CARTESIAN_POINT('Ctrl Pts',(87.3928038273479,-3.83433151573773,3.11253654853231));
#14854=CARTESIAN_POINT('Ctrl Pts',(87.5883866884802,-4.71623267326457,-1.46530803633315));
#14855=CARTESIAN_POINT('Ctrl Pts',(87.7839695496127,-1.39540338501245,-4.73738654552288));
#14856=CARTESIAN_POINT('Ctrl Pts',(87.9795524107449,3.16890048213002,-3.78788314395994));
#14857=CARTESIAN_POINT('Ctrl Pts',(88.1751352718774,4.90932806091437,0.537080847313));
#14858=CARTESIAN_POINT('Ctrl Pts',(88.3707181330097,2.27496153468657,4.38344029191121));
#14859=CARTESIAN_POINT('Ctrl Pts',(88.5663009941421,-2.38668734014466,4.3236280386259));
#14860=CARTESIAN_POINT('Ctrl Pts',(88.7618838552744,-4.92147441756056,0.410938969559601));
#14861=CARTESIAN_POINT('Ctrl Pts',(88.9574667164069,-3.07070813751762,-3.86793931750963));
#14862=CARTESIAN_POINT('Ctrl Pts',(89.1530495775392,1.51657849313516,-4.70003182140403));
#14863=CARTESIAN_POINT('Ctrl Pts',(89.3486324386716,4.75210579955249,-1.34380098470509));
#14864=CARTESIAN_POINT('Ctrl Pts',(89.5442152998039,3.75355745753441,3.20985962464658));
#14865=CARTESIAN_POINT('Ctrl Pts',(89.7397981609363,-0.59113488617187,4.9032686580868));
#14866=CARTESIAN_POINT('Ctrl Pts',(89.9353810220687,-4.40645731763019,2.22702956050341));
#14867=CARTESIAN_POINT('Ctrl Pts',(90.1309638832011,-4.30040573211902,-2.43325837946207));
#14868=CARTESIAN_POINT('Ctrl Pts',(90.3265467443335,-0.351265369080108,
-4.92624390907766));
#14869=CARTESIAN_POINT('Ctrl Pts',(90.4895324619438,3.18025702966254,-3.34307392076952));
#14870=CARTESIAN_POINT('Ctrl Pts',(90.6199663596579,4.30531991685567,-0.727710361102428));
#14871=CARTESIAN_POINT('Ctrl Pts',(90.6852059703279,4.19967249764679,0.682201419182997));
#14872=CARTESIAN_POINT('Ctrl Pts',(90.7178484374759,3.98055747582716,1.33533152506521));
#14873=CARTESIAN_POINT('Ctrl Pts',(82.4467140667525,-1.97444178618949,3.97619622549273));
#14874=CARTESIAN_POINT('Ctrl Pts',(82.4793112102746,-2.6259459695534,3.65268173813828));
#14875=CARTESIAN_POINT('Ctrl Pts',(82.5445054973187,-3.75938060949927,2.67962278220492));
#14876=CARTESIAN_POINT('Ctrl Pts',(82.6748940714069,-4.87749581589017,-0.114325044195209));
#14877=CARTESIAN_POINT('Ctrl Pts',(82.8378797890173,-3.42657633698018,-3.94064929946303));
#14878=CARTESIAN_POINT('Ctrl Pts',(83.0334626501496,1.38836607350325,-5.03669161103426));
#14879=CARTESIAN_POINT('Ctrl Pts',(83.2290455112822,4.95719620937701,-1.63703044387478));
#14880=CARTESIAN_POINT('Ctrl Pts',(83.4246283724142,4.11290814953964,3.21782101801696));
#14881=CARTESIAN_POINT('Ctrl Pts',(83.6202112335468,-0.39859919485411,5.20696839446976));
#14882=CARTESIAN_POINT('Ctrl Pts',(83.815794094679,-4.55386706890918,2.55521669320588));
#14883=CARTESIAN_POINT('Ctrl Pts',(84.0113769558115,-4.65159997492945,-2.37311821348732));
#14884=CARTESIAN_POINT('Ctrl Pts',(84.2069598169438,-0.603947546819121,
-5.18692594548081));
#14885=CARTESIAN_POINT('Ctrl Pts',(84.4025426780763,3.9817727442174,-3.37845640604018));
#14886=CARTESIAN_POINT('Ctrl Pts',(84.5981255392086,5.01931368529363,1.44057511053593));
#14887=CARTESIAN_POINT('Ctrl Pts',(84.7937084003409,1.58401216999367,4.97590499186716));
#14888=CARTESIAN_POINT('Ctrl Pts',(84.9892912614734,-3.26282065364566,4.07709218231267));
#14889=CARTESIAN_POINT('Ctrl Pts',(85.1848741226057,-5.20209424724726,-0.454895075638387));
#14890=CARTESIAN_POINT('Ctrl Pts',(85.3804569837381,-2.5056717476422,-4.58151888068461));
#14891=CARTESIAN_POINT('Ctrl Pts',(85.5760398448705,2.4236044401258,-4.62545604592406));
#14892=CARTESIAN_POINT('Ctrl Pts',(85.7716227060028,5.19315793665816,-0.547555350391454));
#14893=CARTESIAN_POINT('Ctrl Pts',(85.9672055671352,3.33498170761871,4.01828346011176));
#14894=CARTESIAN_POINT('Ctrl Pts',(86.1627884282675,-1.49506477455341,5.00334747678646));
#14895=CARTESIAN_POINT('Ctrl Pts',(86.3583712893999,-4.99282853889391,1.52982623978471));
#14896=CARTESIAN_POINT('Ctrl Pts',(86.5539541505323,-4.04138055467945,-3.30695450892843));
#14897=CARTESIAN_POINT('Ctrl Pts',(86.7495370116647,0.511424314272321,-5.19684039418513));
#14898=CARTESIAN_POINT('Ctrl Pts',(86.9451198727969,4.60848855156075,-2.45571545844803));
#14899=CARTESIAN_POINT('Ctrl Pts',(87.1407027339295,4.59883425653857,2.47374779119925));
#14900=CARTESIAN_POINT('Ctrl Pts',(87.3362855950617,0.491064764562854,5.19880374249346));
#14901=CARTESIAN_POINT('Ctrl Pts',(87.5318684561942,-4.05430284701545,3.29109930593112));
#14902=CARTESIAN_POINT('Ctrl Pts',(87.7274513173265,-4.98679769235471,-1.54937112742509));
#14903=CARTESIAN_POINT('Ctrl Pts',(87.9230341784589,-1.4754561240651,-5.00916513871929));
#14904=CARTESIAN_POINT('Ctrl Pts',(88.1186170395912,3.35069677566378,-4.00518978384787));
#14905=CARTESIAN_POINT('Ctrl Pts',(88.3141999007237,5.1909707474703,0.567892577728663));
#14906=CARTESIAN_POINT('Ctrl Pts',(88.509782761856,2.405473545799,4.63491338249572));
#14907=CARTESIAN_POINT('Ctrl Pts',(88.7053656229884,-2.52360893636046,4.57166976681311));
#14908=CARTESIAN_POINT('Ctrl Pts',(88.9009484841208,-5.20381392707786,0.434514080850038));
#14909=CARTESIAN_POINT('Ctrl Pts',(89.0965313452531,-3.24687124553338,-4.08983869096806));
#14910=CARTESIAN_POINT('Ctrl Pts',(89.2921142063854,1.60358291326754,-4.96966741565522));
#14911=CARTESIAN_POINT('Ctrl Pts',(89.4876970675179,5.0247288199694,-1.42089335148785));
#14912=CARTESIAN_POINT('Ctrl Pts',(89.6832799286502,3.96889487099811,3.39400569859719));
#14913=CARTESIAN_POINT('Ctrl Pts',(89.8788627897826,-0.625047636632337,
5.1845637234469));
#14914=CARTESIAN_POINT('Ctrl Pts',(90.0744456509149,-4.65925086936123,2.35479176760734));
#14915=CARTESIAN_POINT('Ctrl Pts',(90.2700285120473,-4.54711522242937,-2.57285170436789));
#14916=CARTESIAN_POINT('Ctrl Pts',(90.4656113731797,-0.37141707233039,-5.20885703901466));
#14917=CARTESIAN_POINT('Ctrl Pts',(90.62859709079,3.3627048356879,-3.53486235061532));
#14918=CARTESIAN_POINT('Ctrl Pts',(90.7590309885042,4.55231132847466,-0.769458294545144));
#14919=CARTESIAN_POINT('Ctrl Pts',(90.8242705991742,4.44060303441602,0.721338555281245));
#14920=CARTESIAN_POINT('Ctrl Pts',(90.8569130663221,4.20891762767928,1.41193800837531));
#14921=CARTESIAN_POINT('Ctrl Pts',(90.4430005297901,-0.73514273060804,-4.37679816075785));
#14922=CARTESIAN_POINT('Ctrl Pts',(90.4430005297901,-0.604496150119999,
-4.38932450298291));
#14923=CARTESIAN_POINT('Ctrl Pts',(90.4430005297901,-0.473689093681419,
-4.39569210928025));
#14924=CARTESIAN_POINT('Ctrl Pts',(90.4430005297901,-0.343055129970561,
-4.39568396726792));
#14925=CARTESIAN_POINT('Ctrl Pts',(90.4430005297901,-0.334607555765647,
-4.39568344075665));
#14926=CARTESIAN_POINT('Ctrl Pts',(90.4430005297901,-0.32616070523362,-4.39565623476939));
#14927=CARTESIAN_POINT('Ctrl Pts',(90.4430005297901,-0.317714668695276,
-4.39560228305825));
#14928=CARTESIAN_POINT('Ctrl Pts',(90.4430005297901,-0.185997485433182,
-4.39476089818012));
#14929=CARTESIAN_POINT('Ctrl Pts',(90.4430005297901,-0.0544775308798676,
-4.38741913239443));
#14930=CARTESIAN_POINT('Ctrl Pts',(90.4430005297901,0.0764804063629183,
-4.37382331815532));
#14931=CARTESIAN_POINT('Ctrl Pts',(90.4430005297901,0.212139516587092,-4.35973943671001));
#14932=CARTESIAN_POINT('Ctrl Pts',(90.4430005297901,0.347196453096418,-4.33894421155538));
#14933=CARTESIAN_POINT('Ctrl Pts',(90.4430005297901,0.481228112672906,-4.31165627564208));
#14934=CARTESIAN_POINT('Ctrl Pts',(90.4430005297901,0.615259772249436,-4.28436833972878));
#14935=CARTESIAN_POINT('Ctrl Pts',(90.4430005297901,0.748267008612133,-4.2505871487114));
#14936=CARTESIAN_POINT('Ctrl Pts',(90.4430005297901,0.879796089098197,-4.21048338220168));
#14937=CARTESIAN_POINT('Ctrl Pts',(90.4430005297901,0.89695340314272,-4.20525204542176));
#14938=CARTESIAN_POINT('Ctrl Pts',(90.4430005297901,0.914085511767477,-4.19991306416613));
#14939=CARTESIAN_POINT('Ctrl Pts',(90.4430005297901,0.931191357547311,-4.19446676463671));
#14940=CARTESIAN_POINT('Ctrl Pts',(90.4430005297901,0.947772132258861,-4.1891876415421));
#14941=CARTESIAN_POINT('Ctrl Pts',(90.4430005297901,0.964318662466657,-4.18381073214007));
#14942=CARTESIAN_POINT('Ctrl Pts',(90.4430005297901,0.980829620677607,-4.17833682356822));
#14943=CARTESIAN_POINT('Ctrl Pts',(90.4430005297901,1.10554259859385,-4.13699049889617));
#14944=CARTESIAN_POINT('Ctrl Pts',(90.4430005297901,1.22823748709516,-4.09011104027423));
#14945=CARTESIAN_POINT('Ctrl Pts',(90.4430005297901,1.34855752204243,-4.0379369945229));
#14946=CARTESIAN_POINT('Ctrl Pts',(90.4430005297901,1.46900346094926,-3.98570835338396));
#14947=CARTESIAN_POINT('Ctrl Pts',(90.4430005297901,1.58707030868872,-3.9281735359251));
#14948=CARTESIAN_POINT('Ctrl Pts',(90.4430005297901,1.70237501415389,-3.86552606404323));
#14949=CARTESIAN_POINT('Ctrl Pts',(90.4430005297901,1.81579371184005,-3.80390329985934));
#14950=CARTESIAN_POINT('Ctrl Pts',(90.4430005297902,1.9265404734797,-3.73733320231565));
#14951=CARTESIAN_POINT('Ctrl Pts',(90.4430005297902,2.03421675045152,-3.66596377333103));
#14952=CARTESIAN_POINT('Ctrl Pts',(90.4430005297902,2.12284103116633,-3.60722228925794));
#14953=CARTESIAN_POINT('Ctrl Pts',(90.4430005297902,2.2093848220462,-3.5452288234101));
#14954=CARTESIAN_POINT('Ctrl Pts',(90.4430005297902,2.29360397058158,-3.48005089866153));
#14955=CARTESIAN_POINT('Ctrl Pts',(90.4430005297902,2.31916577926078,-3.46026839466446));
#14956=CARTESIAN_POINT('Ctrl Pts',(90.4430005297901,2.34451328416944,-3.44019244944631));
#14957=CARTESIAN_POINT('Ctrl Pts',(90.4430005297901,2.36963923936788,-3.41982474290587));
#14958=CARTESIAN_POINT('Ctrl Pts',(90.4430005297901,2.38341896005211,-3.4086545682841));
#14959=CARTESIAN_POINT('Ctrl Pts',(90.4430005297901,2.39712536031611,-3.3974020346394));
#14960=CARTESIAN_POINT('Ctrl Pts',(90.4430005297901,2.41075460651509,-3.38607005694197));
#14961=CARTESIAN_POINT('Ctrl Pts',(90.4430005297901,2.50863448983006,-3.30468825206748));
#14962=CARTESIAN_POINT('Ctrl Pts',(90.4430005297901,2.60258657057775,-3.21917278388622));
#14963=CARTESIAN_POINT('Ctrl Pts',(90.4430005297901,2.69225999789868,-3.1297002006669));
#14964=CARTESIAN_POINT('Ctrl Pts',(90.4430005297901,2.78082905928829,-3.04132950989942));
#14965=CARTESIAN_POINT('Ctrl Pts',(90.4430005297901,2.86522469916423,-2.94909808560927));
#14966=CARTESIAN_POINT('Ctrl Pts',(90.4430005297901,2.94506902490659,-2.85314508885547));
#14967=CARTESIAN_POINT('Ctrl Pts',(90.4430005297901,3.02294128071918,-2.75956202907352));
#14968=CARTESIAN_POINT('Ctrl Pts',(90.4430005297901,3.09648463049278,-2.66243847701636));
#14969=CARTESIAN_POINT('Ctrl Pts',(90.4430005297901,3.1653041061699,-2.56188124623051));
#14970=CARTESIAN_POINT('Ctrl Pts',(90.4430005297901,3.18089572893538,-2.53909917192192));
#14971=CARTESIAN_POINT('Ctrl Pts',(90.4430005297901,3.19624468510206,-2.51614077549817));
#14972=CARTESIAN_POINT('Ctrl Pts',(90.4430005297901,3.21134602536756,-2.49300717327593));
#14973=CARTESIAN_POINT('Ctrl Pts',(90.4430005297901,3.25596252339905,-2.42465957631677));
#14974=CARTESIAN_POINT('Ctrl Pts',(90.4430005297901,3.29841825709037,-2.35478264430401));
#14975=CARTESIAN_POINT('Ctrl Pts',(90.4430005297901,3.33867108373866,-2.28349579149761));
#14976=CARTESIAN_POINT('Ctrl Pts',(90.4430005297901,3.35066966420011,-2.26224657472299));
#14977=CARTESIAN_POINT('Ctrl Pts',(90.4430005297901,3.3624724508268,-2.24087208124526));
#14978=CARTESIAN_POINT('Ctrl Pts',(90.4430005297901,3.37407817045463,-2.21937547389453));
#14979=CARTESIAN_POINT('Ctrl Pts',(90.4430005297901,3.38411062455509,-2.20079293584626));
#14980=CARTESIAN_POINT('Ctrl Pts',(90.4430005297901,3.39399467672431,-2.18212103945774));
#14981=CARTESIAN_POINT('Ctrl Pts',(90.4430005297901,3.40372092738814,-2.16337919409448));
#14982=CARTESIAN_POINT('Ctrl Pts',(90.4430005297901,3.46057573179043,-2.05382372517903));
#14983=CARTESIAN_POINT('Ctrl Pts',(90.4430005297901,3.5121286929711,-1.94172159775054));
#14984=CARTESIAN_POINT('Ctrl Pts',(90.4430005297901,3.55833134911402,-1.8275194805919));
#14985=CARTESIAN_POINT('Ctrl Pts',(90.4430005297901,3.60477976717121,-1.71270989768844));
#14986=CARTESIAN_POINT('Ctrl Pts',(90.4430005297901,3.64582094812531,-1.59577700537774));
#14987=CARTESIAN_POINT('Ctrl Pts',(90.4430005297901,3.6813548895811,-1.47716007623973));
#14988=CARTESIAN_POINT('Ctrl Pts',(90.4430005297901,3.71649769738405,-1.35984880222698));
#14989=CARTESIAN_POINT('Ctrl Pts',(90.4430005297901,3.74625384223616,-1.24088947957952));
#14990=CARTESIAN_POINT('Ctrl Pts',(90.4430005297901,3.7704762210856,-1.1207062915184));
#14991=CARTESIAN_POINT('Ctrl Pts',(90.4430005297901,3.78454126019077,-1.05092036131019));
#14992=CARTESIAN_POINT('Ctrl Pts',(90.4430005297901,3.79673954198557,-0.980721835780695));
#14993=CARTESIAN_POINT('Ctrl Pts',(90.4430005297901,3.80703431601148,-0.910195398393013));
#14994=CARTESIAN_POINT('Ctrl Pts',(90.4430005297901,3.81275326778125,-0.871016559411345));
#14995=CARTESIAN_POINT('Ctrl Pts',(90.4430005297901,3.81788468776157,-0.831736555533269));
#14996=CARTESIAN_POINT('Ctrl Pts',(90.4430005297901,3.82242148213659,-0.792370186591988));
#14997=CARTESIAN_POINT('Ctrl Pts',(90.4430005297901,3.82477895958205,-0.771914040860601));
#14998=CARTESIAN_POINT('Ctrl Pts',(90.4430005297901,3.82697612959026,-0.751431871386736));
#14999=CARTESIAN_POINT('Ctrl Pts',(90.4430005297901,3.82901104070976,-0.730934968196642));
#15000=CARTESIAN_POINT('Ctrl Pts',(90.4430005297901,3.83052437597814,-0.715691704649243));
#15001=CARTESIAN_POINT('Ctrl Pts',(90.4430005297901,3.83194777392775,-0.700442447857438));
#15002=CARTESIAN_POINT('Ctrl Pts',(90.4430005297901,3.83328081539606,-0.685190377817832));
#15003=CARTESIAN_POINT('Ctrl Pts',(90.4430005297901,3.83425091868927,-0.674090885622473));
#15004=CARTESIAN_POINT('Ctrl Pts',(90.4430005297901,3.83517321726714,-0.662989405527434));
#15005=CARTESIAN_POINT('Ctrl Pts',(90.4430005297901,3.83604763234583,-0.651886262828403));
#15006=CARTESIAN_POINT('Ctrl Pts',(90.4430005297901,3.84560195175947,-0.530567481362801));
#15007=CARTESIAN_POINT('Ctrl Pts',(90.4430005297901,3.84944379016812,-0.409049619730809));
#15008=CARTESIAN_POINT('Ctrl Pts',(90.4430005297901,3.84760828243506,-0.287700070934821));
#15009=CARTESIAN_POINT('Ctrl Pts',(90.4430005297901,3.84578233256279,-0.166982413835497));
#15010=CARTESIAN_POINT('Ctrl Pts',(90.4430005297901,3.83833779215534,-0.0464305624906118));
#15011=CARTESIAN_POINT('Ctrl Pts',(90.4430005297901,3.82525995547212,0.0735799566286457));
#15012=CARTESIAN_POINT('Ctrl Pts',(90.4430005297901,3.82045107309815,0.117709309522672));
#15013=CARTESIAN_POINT('Ctrl Pts',(90.4430005297901,3.81488003307241,0.161765275517719));
#15014=CARTESIAN_POINT('Ctrl Pts',(90.4430005297901,3.80854450228283,0.205728399455354));
#15015=CARTESIAN_POINT('Ctrl Pts',(90.4430005297901,3.80423315264889,0.235645450542401));
#15016=CARTESIAN_POINT('Ctrl Pts',(90.4430005297901,3.79956659035793,0.26552569568798));
#15017=CARTESIAN_POINT('Ctrl Pts',(90.4430005297901,3.79455002103167,0.295328529435823));
#15018=CARTESIAN_POINT('Ctrl Pts',(90.4430005297901,3.77482815796987,0.412493740918343));
#15019=CARTESIAN_POINT('Ctrl Pts',(90.4430005297901,3.74969110989646,0.528545803924548));
#15020=CARTESIAN_POINT('Ctrl Pts',(90.4430005297901,3.7191465886351,0.643128876190501));
#15021=CARTESIAN_POINT('Ctrl Pts',(90.4430005297901,3.68911896816514,0.75577287466225));
#15022=CARTESIAN_POINT('Ctrl Pts',(90.4430005297901,3.65386504693388,0.86699780520124));
#15023=CARTESIAN_POINT('Ctrl Pts',(90.4430005297901,3.61334804281027,0.976442362197689));
#15024=CARTESIAN_POINT('Ctrl Pts',(90.4430005297901,3.58775745474183,1.04556767476729));
#15025=CARTESIAN_POINT('Ctrl Pts',(90.4430005297901,3.56006645269277,1.11398226512644));
#15026=CARTESIAN_POINT('Ctrl Pts',(90.4430005297901,3.5302572329849,1.18158852036477));
#15027=CARTESIAN_POINT('',(82.4415333234128,-2.16533833838417,-3.03088926843041));
#15028=CARTESIAN_POINT('Ctrl Pts',(82.4430005297901,-2.16672251220859,-3.03255290461515));
#15029=CARTESIAN_POINT('Ctrl Pts',(82.4430005297901,-2.2696406448299,-2.97356260115279));
#15030=CARTESIAN_POINT('Ctrl Pts',(82.4430005297901,-2.36930641006408,-2.9095828574348));
#15031=CARTESIAN_POINT('Ctrl Pts',(82.4430005297901,-2.46528951680289,-2.84070661811295));
#15032=CARTESIAN_POINT('Ctrl Pts',(82.4430005297902,-2.55861706129925,-2.77373597600251));
#15033=CARTESIAN_POINT('Ctrl Pts',(82.4430005297901,-2.64846403506778,-2.70213611715619));
#15034=CARTESIAN_POINT('Ctrl Pts',(82.4430005297901,-2.73474523689391,-2.6262943269763));
#15035=CARTESIAN_POINT('Ctrl Pts',(82.4430005297901,-2.7766889505776,-2.58942550427522));
#15036=CARTESIAN_POINT('Ctrl Pts',(82.4430005297901,-2.81778965642945,-2.55155350981108));
#15037=CARTESIAN_POINT('Ctrl Pts',(82.4430005297901,-2.85803541810069,-2.51271907899779));
#15038=CARTESIAN_POINT('Ctrl Pts',(82.4430005297901,-2.8806302377794,-2.49091661023797));
#15039=CARTESIAN_POINT('Ctrl Pts',(82.4430005297901,-2.90295682592989,-2.46880946058695));
#15040=CARTESIAN_POINT('Ctrl Pts',(82.4430005297901,-2.92500922126342,-2.44640821512361));
#15041=CARTESIAN_POINT('Ctrl Pts',(82.4430005297901,-2.94264658870197,-2.4284918395398));
#15042=CARTESIAN_POINT('Ctrl Pts',(82.4430005297901,-2.96010315890421,-2.41039277122427));
#15043=CARTESIAN_POINT('Ctrl Pts',(82.4430005297901,-2.97737164425535,-2.3921219690667));
#15044=CARTESIAN_POINT('Ctrl Pts',(82.4430005297901,-3.05889223068647,-2.30586967327093));
#15045=CARTESIAN_POINT('Ctrl Pts',(82.4430005297901,-3.13626978859535,-2.2157468104726));
#15046=CARTESIAN_POINT('Ctrl Pts',(82.4430005297901,-3.20941666153041,-2.12217282556583));
#15047=CARTESIAN_POINT('Ctrl Pts',(82.4430005297901,-3.28383577531618,-2.02697131180667));
#15048=CARTESIAN_POINT('Ctrl Pts',(82.4430005297901,-3.3538762580029,-1.92819703496745));
#15049=CARTESIAN_POINT('Ctrl Pts',(82.4430005297901,-3.41941495616528,-1.8262468129962));
#15050=CARTESIAN_POINT('Ctrl Pts',(82.4430005297901,-3.44787585716834,-1.78197380702992));
#15051=CARTESIAN_POINT('Ctrl Pts',(82.4430005297901,-3.47548736563765,-1.73710135664425));
#15052=CARTESIAN_POINT('Ctrl Pts',(82.4430005297901,-3.50223725630824,-1.69165980496045));
#15053=CARTESIAN_POINT('Ctrl Pts',(82.4430005297901,-3.51811119609673,-1.66469384595122));
#15054=CARTESIAN_POINT('Ctrl Pts',(82.4430005297901,-3.53368487909068,-1.63752135795755));
#15055=CARTESIAN_POINT('Ctrl Pts',(82.4430005297901,-3.54893402419485,-1.61018817838778));
#15056=CARTESIAN_POINT('Ctrl Pts',(82.4430005297901,-3.6091502173992,-1.50225425746175));
#15057=CARTESIAN_POINT('Ctrl Pts',(82.4430005297901,-3.66437396957584,-1.39171139125269));
#15058=CARTESIAN_POINT('Ctrl Pts',(82.4430005297901,-3.71451260875185,-1.2789963503931));
#15059=CARTESIAN_POINT('Ctrl Pts',(82.4430005297901,-3.76520285462665,-1.16504126048922));
#15060=CARTESIAN_POINT('Ctrl Pts',(82.4430005297901,-3.81069597912495,-1.04886525967351));
#15061=CARTESIAN_POINT('Ctrl Pts',(82.4430005297901,-3.85086009590959,-0.930879705196395));
#15062=CARTESIAN_POINT('Ctrl Pts',(82.4430005297901,-3.89098099755938,-0.81302109890226));
#15063=CARTESIAN_POINT('Ctrl Pts',(82.4430005297901,-3.92578479490074,-0.69335605824151));
#15064=CARTESIAN_POINT('Ctrl Pts',(82.4430005297901,-3.95509723183628,-0.57226596872187));
#15065=CARTESIAN_POINT('Ctrl Pts',(82.4430005297901,-3.97614380137511,-0.485322293750682));
#15066=CARTESIAN_POINT('Ctrl Pts',(82.4430005297901,-3.99435851010471,-0.397643325062507));
#15067=CARTESIAN_POINT('Ctrl Pts',(82.4430005297901,-4.00966125689264,-0.309364507448106));
#15068=CARTESIAN_POINT('Ctrl Pts',(82.4430005297901,-4.01435795168095,-0.282270112673519));
#15069=CARTESIAN_POINT('Ctrl Pts',(82.4430005297901,-4.01878024374387,-0.255119189321616));
#15070=CARTESIAN_POINT('Ctrl Pts',(82.4430005297901,-4.02292554754272,-0.227915601567328));
#15071=CARTESIAN_POINT('Ctrl Pts',(82.4430005297901,-4.02569591908626,-0.20973501721123));
#15072=CARTESIAN_POINT('Ctrl Pts',(82.4430005297901,-4.02834281759651,-0.191528743140453));
#15073=CARTESIAN_POINT('Ctrl Pts',(82.4430005297901,-4.03086308406066,-0.173316124913738));
#15074=CARTESIAN_POINT('Ctrl Pts',(82.4430005297901,-4.04843750869815,-0.046315154568297));
#15075=CARTESIAN_POINT('Ctrl Pts',(82.4430005297901,-4.05988667808791,0.0811706755148063));
#15076=CARTESIAN_POINT('Ctrl Pts',(82.4430005297901,-4.06508069808371,0.208716684251388));
#15077=CARTESIAN_POINT('Ctrl Pts',(82.4430005297901,-4.06928311936486,0.311912679236813));
#15078=CARTESIAN_POINT('Ctrl Pts',(82.4430005297901,-4.06939010282019,0.41514889890651));
#15079=CARTESIAN_POINT('Ctrl Pts',(82.4430005297901,-4.06531043519685,0.518211439887893));
#15080=CARTESIAN_POINT('Ctrl Pts',(82.4430005297901,-4.06037373247765,0.642924816879994));
#15081=CARTESIAN_POINT('Ctrl Pts',(82.4430005297901,-4.04930850365813,0.767384162347736));
#15082=CARTESIAN_POINT('Ctrl Pts',(82.4430005297901,-4.03236186892167,0.891221661938466));
#15083=CARTESIAN_POINT('Ctrl Pts',(82.4430005297901,-4.01541523418522,1.01505916152921));
#15084=CARTESIAN_POINT('Ctrl Pts',(82.4430005297901,-3.99258695128159,1.13827557220802));
#15085=CARTESIAN_POINT('Ctrl Pts',(82.4430005297901,-3.96407180720896,1.26050316969768));
#15086=CARTESIAN_POINT('Ctrl Pts',(82.4430005297901,-3.95547258916303,1.29736294355562));
#15087=CARTESIAN_POINT('Ctrl Pts',(82.4430005297901,-3.9463558470242,1.33413274985256));
#15088=CARTESIAN_POINT('Ctrl Pts',(82.4430005297901,-3.93672603994556,1.37080234332704));
#15089=CARTESIAN_POINT('Ctrl Pts',(82.4430005297901,-3.93229805917785,1.38766376675315));
#15090=CARTESIAN_POINT('Ctrl Pts',(82.4430005297901,-3.92776385858572,1.40449532876003));
#15091=CARTESIAN_POINT('Ctrl Pts',(82.4430005297901,-3.92312493683006,1.42129347051884));
#15092=CARTESIAN_POINT('Ctrl Pts',(82.4430005297901,-3.88922045173421,1.54406604071895));
#15093=CARTESIAN_POINT('Ctrl Pts',(82.4430005297901,-3.84971460164585,1.66509780755738));
#15094=CARTESIAN_POINT('Ctrl Pts',(82.4430005297901,-3.80489648218867,1.78401656475369));
#15095=CARTESIAN_POINT('Ctrl Pts',(82.4430005297901,-3.75909623688204,1.90554125871933));
#15096=CARTESIAN_POINT('Ctrl Pts',(82.4430005297901,-3.70774825330481,2.02486010771724));
#15097=CARTESIAN_POINT('Ctrl Pts',(82.4430005297901,-3.65110614360382,2.14157776456584));
#15098=CARTESIAN_POINT('Ctrl Pts',(82.4430005297901,-3.59646760587821,2.25416682826126));
#15099=CARTESIAN_POINT('Ctrl Pts',(82.4430005297901,-3.53690231336455,2.36433614457288));
#15100=CARTESIAN_POINT('Ctrl Pts',(82.4430005297901,-3.47259286055702,2.47172179522677));
#15101=CARTESIAN_POINT('Ctrl Pts',(82.4430005297901,-3.40566020000046,2.58348774859871));
#15102=CARTESIAN_POINT('Ctrl Pts',(82.4430005297901,-3.33358842352915,2.69223917331592));
#15103=CARTESIAN_POINT('Ctrl Pts',(82.4430005297901,-3.25661397611832,2.79770775568241));
#15104=CARTESIAN_POINT('Ctrl Pts',(82.4430005297901,-3.24591769429999,2.81236355014301));
#15105=CARTESIAN_POINT('Ctrl Pts',(82.4430005297901,-3.23512667474305,2.82695590898394));
#15106=CARTESIAN_POINT('Ctrl Pts',(82.4430005297901,-3.22424148623506,2.8414840661082));
#15107=CARTESIAN_POINT('Ctrl Pts',(82.4430005297901,-3.19678203985352,2.87813342236721));
#15108=CARTESIAN_POINT('Ctrl Pts',(82.4430005297901,-3.16876263224132,2.91432166979658));
#15109=CARTESIAN_POINT('Ctrl Pts',(82.4430005297901,-3.14020380828486,2.95003182240799));
#15110=CARTESIAN_POINT('Ctrl Pts',(82.4430005297901,-3.05724825873483,3.05376002000154));
#15111=CARTESIAN_POINT('Ctrl Pts',(82.4430005297901,-2.96972905213257,3.15347708428787));
#15112=CARTESIAN_POINT('Ctrl Pts',(82.4430005297901,-2.87797244189919,3.24894641929633));
#15113=CARTESIAN_POINT('Ctrl Pts',(82.4430005297901,-2.78576185253439,3.34488810268026));
#15114=CARTESIAN_POINT('Ctrl Pts',(82.4430005297901,-2.68927141017721,3.43654055759438));
#15115=CARTESIAN_POINT('Ctrl Pts',(82.4430005297901,-2.58878423218922,3.52364130332058));
#15116=CARTESIAN_POINT('Ctrl Pts',(82.4430005297901,-2.48907040233302,3.61007172273917));
#15117=CARTESIAN_POINT('Ctrl Pts',(82.4430005297901,-2.38542062149339,3.69202080476271));
#15118=CARTESIAN_POINT('Ctrl Pts',(82.4430005297901,-2.27807132967477,3.7692010985491));
#15119=CARTESIAN_POINT('Ctrl Pts',(82.4430005297901,-2.18508355965287,3.83605597283143));
#15120=CARTESIAN_POINT('Ctrl Pts',(82.4430005297901,-2.08931913384727,3.89933243962664));
#15121=CARTESIAN_POINT('Ctrl Pts',(82.4430005297901,-1.99091130097234,3.9588194824242));
#15122=CARTESIAN_POINT('Ctrl Pts',(82.4430005297901,-1.98447919887495,3.96270765597266));
#15123=CARTESIAN_POINT('Ctrl Pts',(82.4430005297901,-1.97803579776514,3.96657963149843));
#15124=CARTESIAN_POINT('Ctrl Pts',(82.4430005297901,-1.97158113240047,3.97043534620103));
#15125=CARTESIAN_POINT('Ctrl Pts',(82.4415333234128,-2.16408072405065,-3.02912894778225));
#15126=CARTESIAN_POINT('Ctrl Pts',(82.4420336965111,-2.15504512285644,-3.03558419307279));
#15127=CARTESIAN_POINT('Ctrl Pts',(82.4425340696094,-2.14598063840387,-3.04199900959491));
#15128=CARTESIAN_POINT('Ctrl Pts',(82.4430344427077,-2.13688763362806,-3.04837314050421));
#15129=CARTESIAN_POINT('Ctrl Pts',(82.0310032950812,2.5732449024852,-3.61351950356445));
#15130=CARTESIAN_POINT('Ctrl Pts',(82.0636457680076,3.16616325925722,-3.19130979057643));
#15131=CARTESIAN_POINT('Ctrl Pts',(82.1288853844562,4.13207912470726,-2.05174262577274));
#15132=CARTESIAN_POINT('Ctrl Pts',(82.2593192879487,4.79464520668388,0.882555540610264));
#15133=CARTESIAN_POINT('Ctrl Pts',(82.4223050055592,2.75914274104666,4.42905501007769));
#15134=CARTESIAN_POINT('Ctrl Pts',(82.6178878666914,-2.16479008544544,4.75065483431134));
#15135=CARTESIAN_POINT('Ctrl Pts',(82.8134707278238,-5.14967299145611,0.832949191282387));
#15136=CARTESIAN_POINT('Ctrl Pts',(83.0090535889562,-3.55042897662582,-3.82414592282758));
#15137=CARTESIAN_POINT('Ctrl Pts',(83.2046364500884,1.21504830394734,-5.0748705164238));
#15138=CARTESIAN_POINT('Ctrl Pts',(83.400219311221,4.89660859864141,-1.80258629906098));
#15139=CARTESIAN_POINT('Ctrl Pts',(83.5958021723532,4.21527029670854,3.07568249282053));
#15140=CARTESIAN_POINT('Ctrl Pts',(83.7913850334858,-0.222660655853561,
5.21331275103613));
#15141=CARTESIAN_POINT('Ctrl Pts',(83.9869678946179,-4.46203744762071,2.7051724468734));
#15142=CARTESIAN_POINT('Ctrl Pts',(84.1825507557504,-4.72526831706301,-2.21356276749624));
#15143=CARTESIAN_POINT('Ctrl Pts',(84.3781336168827,-0.777683074796472,
-5.15976630774078));
#15144=CARTESIAN_POINT('Ctrl Pts',(84.5737164780151,3.86289539882142,-3.50798698251897));
#15145=CARTESIAN_POINT('Ctrl Pts',(84.7692993391475,5.06117659898468,1.26982667827935));
#15146=CARTESIAN_POINT('Ctrl Pts',(84.96488220028,1.74933589258655,4.91607408021796));
#15147=CARTESIAN_POINT('Ctrl Pts',(85.1604650614123,-3.12137193940479,4.18150613925552));
#15148=CARTESIAN_POINT('Ctrl Pts',(85.3560479225446,-5.21056228074381,-0.279286952965116));
#15149=CARTESIAN_POINT('Ctrl Pts',(85.5516307836769,-2.65651348040282,-4.49120199383985));
#15150=CARTESIAN_POINT('Ctrl Pts',(85.7472136448093,2.26480862632819,-4.70091489012678));
#15151=CARTESIAN_POINT('Ctrl Pts',(85.9427965059417,5.16791352719978,-0.721546383514633));
#15152=CARTESIAN_POINT('Ctrl Pts',(86.1383793670741,3.46578485734584,3.90080690363208));
#15153=CARTESIAN_POINT('Ctrl Pts',(86.3339622282066,-1.32477558834876,5.04707131090363));
#15154=CARTESIAN_POINT('Ctrl Pts',(86.5295450893389,-4.93480143762726,1.69578718575462));
#15155=CARTESIAN_POINT('Ctrl Pts',(86.7251279504711,-4.14732466254241,-3.16664760615603));
#15156=CARTESIAN_POINT('Ctrl Pts',(86.9207108116036,0.335917868796414,-5.20721791424714));
#15157=CARTESIAN_POINT('Ctrl Pts',(87.1162936727359,4.51981737154225,-2.60752975275673));
#15158=CARTESIAN_POINT('Ctrl Pts',(87.3118765338683,4.67601458569188,2.3157815033228));
#15159=CARTESIAN_POINT('Ctrl Pts',(87.5074593950007,0.665320577523391,5.17545253638813));
#15160=CARTESIAN_POINT('Ctrl Pts',(87.7030422561331,-3.93825640509612,3.42317175243948));
#15161=CARTESIAN_POINT('Ctrl Pts',(87.8986251172654,-5.03236803225271,-1.37956714940564));
#15162=CARTESIAN_POINT('Ctrl Pts',(88.0942079783978,-1.64204264387256,-4.95294612034352));
#15163=CARTESIAN_POINT('Ctrl Pts',(88.2897908395301,3.21155918647893,-4.11265223251709));
#15164=CARTESIAN_POINT('Ctrl Pts',(88.4853737006626,5.20323685809616,0.39250777042273));
#15165=CARTESIAN_POINT('Ctrl Pts',(88.6809565617948,2.55828132447017,4.54790108430783));
#15166=CARTESIAN_POINT('Ctrl Pts',(88.8765394229273,-2.36656955065493,4.65055642185629));
#15167=CARTESIAN_POINT('Ctrl Pts',(89.0721222840597,-5.1821983422279,0.609026662521216));
#15168=CARTESIAN_POINT('Ctrl Pts',(89.2677051451921,-3.38052451202556,-3.97526189866621));
#15169=CARTESIAN_POINT('Ctrl Pts',(89.4632880063243,1.43495189680254,-5.01702611225074));
#15170=CARTESIAN_POINT('Ctrl Pts',(89.6588708674568,4.96896142408185,-1.58819351471315));
#15171=CARTESIAN_POINT('Ctrl Pts',(89.8544537285891,4.08065273654629,3.25627251816026));
#15172=CARTESIAN_POINT('Ctrl Pts',(90.0500365897215,-0.455561874102168,
5.19825550801701));
#15173=CARTESIAN_POINT('Ctrl Pts',(90.2130223073318,-3.87588474101625,2.95720212609757));
#15174=CARTESIAN_POINT('Ctrl Pts',(90.3434108814201,-4.6129921626674,0.0418147320781305));
#15175=CARTESIAN_POINT('Ctrl Pts',(90.4086051684642,-4.26823548650425,-1.41053445637093));
#15176=CARTESIAN_POINT('Ctrl Pts',(90.4412023119862,-3.93156634387324,-2.05472598388759));
#15177=CARTESIAN_POINT('Ctrl Pts',(82.1694296294366,2.43416713531397,-3.41821736823327));
#15178=CARTESIAN_POINT('Ctrl Pts',(82.202072102363,2.99503966500787,-3.01882708611391));
#15179=CARTESIAN_POINT('Ctrl Pts',(82.2673117188115,3.9087500751154,-1.94085081639738));
#15180=CARTESIAN_POINT('Ctrl Pts',(82.3977456223042,4.53550603610597,0.834855512574021));
#15181=CARTESIAN_POINT('Ctrl Pts',(82.5607313399144,2.61001763781187,4.18967512016311));
#15182=CARTESIAN_POINT('Ctrl Pts',(82.7563142010469,-2.04778832972938,4.49389323874026));
#15183=CARTESIAN_POINT('Ctrl Pts',(82.9518970621792,-4.8713454134545,0.787930268451231));
#15184=CARTESIAN_POINT('Ctrl Pts',(83.1474799233117,-3.3585367342309,-3.61745993045656));
#15185=CARTESIAN_POINT('Ctrl Pts',(83.3430627844438,1.14937783280214,-4.80058583429903));
#15186=CARTESIAN_POINT('Ctrl Pts',(83.5386456455763,4.63195854922217,-1.70516079658948));
#15187=CARTESIAN_POINT('Ctrl Pts',(83.7342285067087,3.98744496211903,2.90944916881162));
#15188=CARTESIAN_POINT('Ctrl Pts',(83.9298113678411,-0.210626376946379,
4.93154559538018));
#15189=CARTESIAN_POINT('Ctrl Pts',(84.1253942289734,-4.22087493539727,2.55896430968406));
#15190=CARTESIAN_POINT('Ctrl Pts',(84.3209770901058,-4.46987880237384,-2.09392496430875));
#15191=CARTESIAN_POINT('Ctrl Pts',(84.5165599512381,-0.735651154124987,
-4.88089320999837));
#15192=CARTESIAN_POINT('Ctrl Pts',(84.7121428123705,3.6541150894287,-3.31838862896805));
#15193=CARTESIAN_POINT('Ctrl Pts',(84.9077256735029,4.78763204053,1.20119556627793));
#15194=CARTESIAN_POINT('Ctrl Pts',(85.1033085346353,1.65478844794245,4.65037196781321));
#15195=CARTESIAN_POINT('Ctrl Pts',(85.2988913957676,-2.95266920946872,3.95550567707689));
#15196=CARTESIAN_POINT('Ctrl Pts',(85.4944742569001,-4.92894378146587,-0.264192157370293));
#15197=CARTESIAN_POINT('Ctrl Pts',(85.6900571180323,-2.51293524462826,-4.24846320725372));
#15198=CARTESIAN_POINT('Ctrl Pts',(85.8856399791648,2.14240110634607,-4.44684162024508));
#15199=CARTESIAN_POINT('Ctrl Pts',(86.0812228402971,4.88860009162169,-0.682548517500101));
#15200=CARTESIAN_POINT('Ctrl Pts',(86.2768057014295,3.27846742829351,3.6899775675672));
#15201=CARTESIAN_POINT('Ctrl Pts',(86.4723885625619,-1.25317461844009,4.7742891097239));
#15202=CARTESIAN_POINT('Ctrl Pts',(86.6679714236942,-4.6680871560928,1.60413392136281));
#15203=CARTESIAN_POINT('Ctrl Pts',(86.8635542848266,-3.92317162788817,-2.9954978341087));
#15204=CARTESIAN_POINT('Ctrl Pts',(87.0591371459591,0.31776230688313,-4.92578017002461));
#15205=CARTESIAN_POINT('Ctrl Pts',(87.2547200070913,4.27553199184569,-2.46659897096611));
#15206=CARTESIAN_POINT('Ctrl Pts',(87.4503028682238,4.42328711804585,2.19061902056514));
#15207=CARTESIAN_POINT('Ctrl Pts',(87.645885729356,0.62936158260391,4.89573163529303));
#15208=CARTESIAN_POINT('Ctrl Pts',(87.8414685904886,-3.72540301254123,3.23815746036292));
#15209=CARTESIAN_POINT('Ctrl Pts',(88.0370514516208,-4.76038050831605,-1.30500482592964));
#15210=CARTESIAN_POINT('Ctrl Pts',(88.2326343127533,-1.55329414415176,-4.68525116186073));
#15211=CARTESIAN_POINT('Ctrl Pts',(88.4282171738855,3.03798205032592,-3.89037316024618));
#15212=CARTESIAN_POINT('Ctrl Pts',(88.623800035018,4.92201428049067,0.371293658911228));
#15213=CARTESIAN_POINT('Ctrl Pts',(88.8193828961503,2.42001230310359,4.30209784672624));
#15214=CARTESIAN_POINT('Ctrl Pts',(89.0149657572827,-2.23866209472541,4.39920490741982));
#15215=CARTESIAN_POINT('Ctrl Pts',(89.2105486184151,-4.90211284637034,0.576110219826852));
#15216=CARTESIAN_POINT('Ctrl Pts',(89.4061314795474,-3.19781520186777,-3.760408447192));
#15217=CARTESIAN_POINT('Ctrl Pts',(89.6017143406798,1.35739615944824,-4.74586778260333));
#15218=CARTESIAN_POINT('Ctrl Pts',(89.7972972018122,4.70040087652035,-1.50235543235697));
#15219=CARTESIAN_POINT('Ctrl Pts',(89.9928800629445,3.86010316092995,3.08027873276914));
#15220=CARTESIAN_POINT('Ctrl Pts',(90.188462924077,-0.430939838244923,4.91730216053644));
#15221=CARTESIAN_POINT('Ctrl Pts',(90.3514486416872,-3.66640238856974,2.79737238413463));
#15222=CARTESIAN_POINT('Ctrl Pts',(90.4818372157755,-4.36367090710306,0.0395547452550024));
#15223=CARTESIAN_POINT('Ctrl Pts',(90.5470315028196,-4.03754750937051,-1.33429842360129));
#15224=CARTESIAN_POINT('Ctrl Pts',(90.5796286463417,-3.71907453321684,-1.94367293110128));
#15225=CARTESIAN_POINT('Ctrl Pts',(82.307855963792,2.29508936814274,-3.22291523290208));
#15226=CARTESIAN_POINT('Ctrl Pts',(82.3404984367184,2.82391607075853,-2.84634438165137));
#15227=CARTESIAN_POINT('Ctrl Pts',(82.4057380531669,3.68542102552352,-1.82995900702202));
#15228=CARTESIAN_POINT('Ctrl Pts',(82.5361719566594,4.27636686552807,0.787155484537778));
#15229=CARTESIAN_POINT('Ctrl Pts',(82.6991576742698,2.46089253457709,3.95029523024854));
#15230=CARTESIAN_POINT('Ctrl Pts',(82.8947405354022,-1.93078657401334,4.23713164316919));
#15231=CARTESIAN_POINT('Ctrl Pts',(83.0903233965346,-4.59301783545288,0.742911345620072));
#15232=CARTESIAN_POINT('Ctrl Pts',(83.2859062576669,-3.16664449183598,-3.41077393808554));
#15233=CARTESIAN_POINT('Ctrl Pts',(83.4814891187993,1.08370736165695,-4.52630115217425));
#15234=CARTESIAN_POINT('Ctrl Pts',(83.6770719799316,4.36730849980295,-1.60773529411797));
#15235=CARTESIAN_POINT('Ctrl Pts',(83.8726548410641,3.75961962752953,2.7432158448027));
#15236=CARTESIAN_POINT('Ctrl Pts',(84.0682377021964,-0.198592098039204,
4.64977843972425));
#15237=CARTESIAN_POINT('Ctrl Pts',(84.2638205633287,-3.97971242317383,2.41275617249475));
#15238=CARTESIAN_POINT('Ctrl Pts',(84.4594034244612,-4.21448928768466,-1.97428716112127));
#15239=CARTESIAN_POINT('Ctrl Pts',(84.6549862855934,-0.693619233453502,
-4.60202011225595));
#15240=CARTESIAN_POINT('Ctrl Pts',(84.8505691467259,3.44533478003599,-3.12879027541714));
#15241=CARTESIAN_POINT('Ctrl Pts',(85.0461520078582,4.51408748207532,1.13256445427651));
#15242=CARTESIAN_POINT('Ctrl Pts',(85.2417348689906,1.56024100329834,4.38466985540846));
#15243=CARTESIAN_POINT('Ctrl Pts',(85.437317730123,-2.78396647953264,3.72950521489826));
#15244=CARTESIAN_POINT('Ctrl Pts',(85.6329005912553,-4.64732528218793,-0.249097361775471));
#15245=CARTESIAN_POINT('Ctrl Pts',(85.8284834523878,-2.36935700885369,-4.00572442066759));
#15246=CARTESIAN_POINT('Ctrl Pts',(86.02406631352,2.01999358636394,-4.19276835036339));
#15247=CARTESIAN_POINT('Ctrl Pts',(86.2196491746525,4.60928665604361,-0.643550651485564));
#15248=CARTESIAN_POINT('Ctrl Pts',(86.4152320357848,3.09114999924119,3.47914823150234));
#15249=CARTESIAN_POINT('Ctrl Pts',(86.6108148969172,-1.18157364853143,4.50150690854415));
#15250=CARTESIAN_POINT('Ctrl Pts',(86.8063977580496,-4.40137287455832,1.512480656971));
#15251=CARTESIAN_POINT('Ctrl Pts',(87.0019806191819,-3.69901859323395,-2.82434806206138));
#15252=CARTESIAN_POINT('Ctrl Pts',(87.1975634803144,0.299606744969849,-4.6443424258021));
#15253=CARTESIAN_POINT('Ctrl Pts',(87.3931463414466,4.03124661214913,-2.3256681891755));
#15254=CARTESIAN_POINT('Ctrl Pts',(87.5887292025792,4.17055965039982,2.06545653780747));
#15255=CARTESIAN_POINT('Ctrl Pts',(87.7843120637113,0.593402587684435,4.61601073419793));
#15256=CARTESIAN_POINT('Ctrl Pts',(87.9798949248439,-3.51254961998634,3.05314316828636));
#15257=CARTESIAN_POINT('Ctrl Pts',(88.1754777859761,-4.48839298437938,-1.23044250245362));
#15258=CARTESIAN_POINT('Ctrl Pts',(88.3710606471085,-1.46454564443096,-4.41755620337796));
#15259=CARTESIAN_POINT('Ctrl Pts',(88.566643508241,2.8644049141729,-3.66809408797527));
#15260=CARTESIAN_POINT('Ctrl Pts',(88.7622263693732,4.64079170288519,0.350079547399718));
#15261=CARTESIAN_POINT('Ctrl Pts',(88.9578092305058,2.28174328173701,4.05629460914468));
#15262=CARTESIAN_POINT('Ctrl Pts',(89.1533920916379,-2.11075463879587,4.14785339298334));
#15263=CARTESIAN_POINT('Ctrl Pts',(89.3489749527706,-4.62202735051278,0.543193777132494));
#15264=CARTESIAN_POINT('Ctrl Pts',(89.5445578139026,-3.01510589170997,-3.54555499571779));
#15265=CARTESIAN_POINT('Ctrl Pts',(89.7401406750352,1.27984042209396,-4.47470945295592));
#15266=CARTESIAN_POINT('Ctrl Pts',(89.9357235361675,4.43184032895884,-1.41651735000079));
#15267=CARTESIAN_POINT('Ctrl Pts',(90.1313063972999,3.6395535853136,2.90428494737804));
#15268=CARTESIAN_POINT('Ctrl Pts',(90.3268892584322,-0.406317802387683,
4.63634881305585));
#15269=CARTESIAN_POINT('Ctrl Pts',(90.4898749760426,-3.45692003612324,2.63754264217168));
#15270=CARTESIAN_POINT('Ctrl Pts',(90.6202635501308,-4.11434965153871,0.0372947584318718));
#15271=CARTESIAN_POINT('Ctrl Pts',(90.6854578371749,-3.80685953223677,-1.25806239083166));
#15272=CARTESIAN_POINT('Ctrl Pts',(90.718054980697,-3.50658272256043,-1.83261987831497));
#15273=CARTESIAN_POINT('Ctrl Pts',(82.4462822981473,2.15601160097152,-3.0276130975709));
#15274=CARTESIAN_POINT('Ctrl Pts',(82.4789247710738,2.65279247650918,-2.67386167718884));
#15275=CARTESIAN_POINT('Ctrl Pts',(82.5441643875223,3.46209197593166,-1.71906719764665));
#15276=CARTESIAN_POINT('Ctrl Pts',(82.6745982910148,4.01722769495016,0.739455456501537));
#15277=CARTESIAN_POINT('Ctrl Pts',(82.8375840086252,2.3117674313423,3.71091534033396));
#15278=CARTESIAN_POINT('Ctrl Pts',(83.0331668697575,-1.81378481829728,3.98037004759811));
#15279=CARTESIAN_POINT('Ctrl Pts',(83.2287497308899,-4.31469025745127,0.697892422788916));
#15280=CARTESIAN_POINT('Ctrl Pts',(83.4243325920222,-2.97475224944107,-3.20408794571452));
#15281=CARTESIAN_POINT('Ctrl Pts',(83.6199154531546,1.01803689051175,-4.25201647004949));
#15282=CARTESIAN_POINT('Ctrl Pts',(83.815498314287,4.10265845038372,-1.51030979164646));
#15283=CARTESIAN_POINT('Ctrl Pts',(84.0110811754194,3.53179429294001,2.57698252079379));
#15284=CARTESIAN_POINT('Ctrl Pts',(84.2066640365517,-0.186557819132022,
4.3680112840683));
#15285=CARTESIAN_POINT('Ctrl Pts',(84.4022468976841,-3.73854991095039,2.26654803530542));
#15286=CARTESIAN_POINT('Ctrl Pts',(84.5978297588165,-3.95909977299548,-1.85464935793378));
#15287=CARTESIAN_POINT('Ctrl Pts',(84.7934126199488,-0.651587312782014,
-4.32314701451353));
#15288=CARTESIAN_POINT('Ctrl Pts',(84.9889954810813,3.23655447064327,-2.93919192186622));
#15289=CARTESIAN_POINT('Ctrl Pts',(85.1845783422135,4.24054292362064,1.06393334227509));
#15290=CARTESIAN_POINT('Ctrl Pts',(85.380161203346,1.46569355865423,4.11896774300371));
#15291=CARTESIAN_POINT('Ctrl Pts',(85.5757440644783,-2.61526374959657,3.50350475271963));
#15292=CARTESIAN_POINT('Ctrl Pts',(85.7713269256107,-4.36570678291,-0.234002566180649));
#15293=CARTESIAN_POINT('Ctrl Pts',(85.966909786743,-2.22577877307914,-3.76298563408145));
#15294=CARTESIAN_POINT('Ctrl Pts',(86.1624926478755,1.89758606638183,-3.93869508048168));
#15295=CARTESIAN_POINT('Ctrl Pts',(86.3580755090077,4.32997322046552,-0.604552785471028));
#15296=CARTESIAN_POINT('Ctrl Pts',(86.5536583701403,2.90383257018886,3.26831889543747));
#15297=CARTESIAN_POINT('Ctrl Pts',(86.7492412312724,-1.10997267862275,4.22872470736441));
#15298=CARTESIAN_POINT('Ctrl Pts',(86.944824092405,-4.13465859302386,1.42082739257919));
#15299=CARTESIAN_POINT('Ctrl Pts',(87.1404069535373,-3.47486555857972,-2.65319829001405));
#15300=CARTESIAN_POINT('Ctrl Pts',(87.3359898146697,0.281451183056565,-4.36290468157959));
#15301=CARTESIAN_POINT('Ctrl Pts',(87.5315726758021,3.78696123245258,-2.18473740738487));
#15302=CARTESIAN_POINT('Ctrl Pts',(87.7271555369346,3.91783218275379,1.9402940550498));
#15303=CARTESIAN_POINT('Ctrl Pts',(87.9227383980667,0.557443592764954,4.33628983310282));
#15304=CARTESIAN_POINT('Ctrl Pts',(88.1183212591992,-3.29969622743145,2.8681288762098));
#15305=CARTESIAN_POINT('Ctrl Pts',(88.3139041203315,-4.21640546044272,-1.15588017897761));
#15306=CARTESIAN_POINT('Ctrl Pts',(88.5094869814639,-1.37579714471017,-4.14986124489519));
#15307=CARTESIAN_POINT('Ctrl Pts',(88.7050698425962,2.69082777801989,-3.44581501570436));
#15308=CARTESIAN_POINT('Ctrl Pts',(88.9006527037287,4.3595691252797,0.328865435888209));
#15309=CARTESIAN_POINT('Ctrl Pts',(89.096235564861,2.14347426037042,3.8104913715631));
#15310=CARTESIAN_POINT('Ctrl Pts',(89.2918184259934,-1.98284718286635,3.89650187854686));
#15311=CARTESIAN_POINT('Ctrl Pts',(89.4874012871258,-4.34194185465522,0.510277334438133));
#15312=CARTESIAN_POINT('Ctrl Pts',(89.6829841482581,-2.83239658155217,-3.33070154424358));
#15313=CARTESIAN_POINT('Ctrl Pts',(89.8785670093905,1.20228468473967,-4.20355112330852));
#15314=CARTESIAN_POINT('Ctrl Pts',(90.0741498705228,4.16327978139733,-1.3306792676446));
#15315=CARTESIAN_POINT('Ctrl Pts',(90.2697327316552,3.41900400969726,2.72829116198692));
#15316=CARTESIAN_POINT('Ctrl Pts',(90.4653155927876,-0.381695766530438,
4.35539546557527));
#15317=CARTESIAN_POINT('Ctrl Pts',(90.6283013103979,-3.24743768367674,2.47771290020874));
#15318=CARTESIAN_POINT('Ctrl Pts',(90.7586898844862,-3.86502839597435,0.035034771608743));
#15319=CARTESIAN_POINT('Ctrl Pts',(90.8238841715303,-3.57617155510303,-1.18182635806204));
#15320=CARTESIAN_POINT('Ctrl Pts',(90.8564813150523,-3.29409091190402,-1.72156682552866));
#15321=CARTESIAN_POINT('',(90.4444676558701,0.0297160312282678,3.7247948877017));
#15322=CARTESIAN_POINT('Ctrl Pts',(90.4430005297901,0.0295740726440573,
3.72695441077287));
#15323=CARTESIAN_POINT('Ctrl Pts',(90.4430005297901,-0.0884458352819756,
3.73973311544784));
#15324=CARTESIAN_POINT('Ctrl Pts',(90.4430005297901,-0.206685143677292,
3.7465459652833));
#15325=CARTESIAN_POINT('Ctrl Pts',(90.4430005297901,-0.324736322595995,
3.74724091818272));
#15326=CARTESIAN_POINT('Ctrl Pts',(90.4430005297901,-0.439290627898788,
3.74791528541344));
#15327=CARTESIAN_POINT('Ctrl Pts',(90.4430005297901,-0.55366870084768,3.74282988407892));
#15328=CARTESIAN_POINT('Ctrl Pts',(90.4430005297901,-0.66757511375052,3.73226995515168));
#15329=CARTESIAN_POINT('Ctrl Pts',(90.4430005297901,-0.784700158626253,
3.72141163630932));
#15330=CARTESIAN_POINT('Ctrl Pts',(90.4430005297901,-0.901327146820539,
3.70476502258063));
#15331=CARTESIAN_POINT('Ctrl Pts',(90.4430005297901,-1.01714336497883,3.68258477181881));
#15332=CARTESIAN_POINT('Ctrl Pts',(90.4430005297901,-1.13295958313712,3.660404521057));
#15333=CARTESIAN_POINT('Ctrl Pts',(90.4430005297901,-1.24796575142807,3.63269035768899));
#15334=CARTESIAN_POINT('Ctrl Pts',(90.4430005297901,-1.36184717318807,3.59964481501032));
#15335=CARTESIAN_POINT('Ctrl Pts',(90.4430005297901,-1.37934384898826,3.59456771693801));
#15336=CARTESIAN_POINT('Ctrl Pts',(90.4430005297901,-1.39681395895271,3.58936467583837));
#15337=CARTESIAN_POINT('Ctrl Pts',(90.4430005297901,-1.41425634058429,3.584036323652));
#15338=CARTESIAN_POINT('Ctrl Pts',(90.4430005297901,-1.43024624853253,3.57915167757696));
#15339=CARTESIAN_POINT('Ctrl Pts',(90.4430005297901,-1.44620373585888,3.57416449842206));
#15340=CARTESIAN_POINT('Ctrl Pts',(90.4430005297901,-1.46212623027145,3.56907619712215));
#15341=CARTESIAN_POINT('Ctrl Pts',(90.4430005297901,-1.57724288748944,3.53228873019729));
#15342=CARTESIAN_POINT('Ctrl Pts',(90.4430005297901,-1.69055927763167,3.49021107252789));
#15343=CARTESIAN_POINT('Ctrl Pts',(90.4430005297901,-1.80175485570888,3.44314758727645));
#15344=CARTESIAN_POINT('Ctrl Pts',(90.4430005297901,-1.91486434019661,3.3952740418798));
#15345=CARTESIAN_POINT('Ctrl Pts',(90.4430005297901,-2.02578012661322,3.34224138479951));
#15346=CARTESIAN_POINT('Ctrl Pts',(90.4430005297901,-2.13416539498154,3.28431509258683));
#15347=CARTESIAN_POINT('Ctrl Pts',(90.4430005297901,-2.2433349494361,3.22596964022727));
#15348=CARTESIAN_POINT('Ctrl Pts',(90.4430005297901,-2.34993804867473,3.16265919293307));
#15349=CARTESIAN_POINT('Ctrl Pts',(90.4430005297901,-2.45361918023358,3.09460343027293));
#15350=CARTESIAN_POINT('Ctrl Pts',(90.4430005297901,-2.50781789043285,3.05902767504775));
#15351=CARTESIAN_POINT('Ctrl Pts',(90.4430005297901,-2.56121787735912,3.02215438256582));
#15352=CARTESIAN_POINT('Ctrl Pts',(90.4430005297901,-2.61376597529677,2.98400978512265));
#15353=CARTESIAN_POINT('Ctrl Pts',(90.4430005297901,-2.64845254685223,2.95883084695753));
#15354=CARTESIAN_POINT('Ctrl Pts',(90.4430005297901,-2.68276789522009,2.93309790327227));
#15355=CARTESIAN_POINT('Ctrl Pts',(90.4430005297901,-2.7166962006516,2.90681771213872));
#15356=CARTESIAN_POINT('Ctrl Pts',(90.4430005297901,-2.74521796869836,2.88472531741983));
#15357=CARTESIAN_POINT('Ctrl Pts',(90.4430005297901,-2.77347318832931,2.86223997607677));
#15358=CARTESIAN_POINT('Ctrl Pts',(90.4430005297901,-2.8013972675781,2.83941177244806));
#15359=CARTESIAN_POINT('Ctrl Pts',(90.4430005297901,-2.89986803616091,2.75891097109109));
#15360=CARTESIAN_POINT('Ctrl Pts',(90.4430005297901,-2.99436179703228,2.67404616107294));
#15361=CARTESIAN_POINT('Ctrl Pts',(90.4430005297901,-3.08452940138303,2.58509397524089));
#15362=CARTESIAN_POINT('Ctrl Pts',(90.4430005297901,-3.17439015065303,2.49644450822192));
#15363=CARTESIAN_POINT('Ctrl Pts',(90.4430005297901,-3.25995494461917,2.40373502869822));
#15364=CARTESIAN_POINT('Ctrl Pts',(90.4430005297901,-3.34085919834289,2.30719182178546));
#15365=CARTESIAN_POINT('Ctrl Pts',(90.4430005297901,-3.41877281360875,2.21421734969377));
#15366=CARTESIAN_POINT('Ctrl Pts',(90.4430005297901,-3.49236462902197,2.11768677390185));
#15367=CARTESIAN_POINT('Ctrl Pts',(90.4430005297901,-3.56128171283005,2.01776553973379));
#15368=CARTESIAN_POINT('Ctrl Pts',(90.4430005297901,-3.57213897168619,2.0020238593747));
#15369=CARTESIAN_POINT('Ctrl Pts',(90.4430005297901,-3.58288014117297,1.98619795895379));
#15370=CARTESIAN_POINT('Ctrl Pts',(90.4430005297901,-3.59350376280769,1.97028841204379));
#15371=CARTESIAN_POINT('Ctrl Pts',(90.4430005297901,-3.65258853086704,1.88180522604296));
#15372=CARTESIAN_POINT('Ctrl Pts',(90.4430005297901,-3.70803921479689,1.79073595284716));
#15373=CARTESIAN_POINT('Ctrl Pts',(90.4430005297901,-3.75982007731666,1.6973347500856));
#15374=CARTESIAN_POINT('Ctrl Pts',(90.4430005297901,-3.76811332474679,1.68237556927864));
#15375=CARTESIAN_POINT('Ctrl Pts',(90.4430005297901,-3.77631159693478,1.66735785530936));
#15376=CARTESIAN_POINT('Ctrl Pts',(90.4430005297901,-3.78440902583728,1.65229362110776));
#15377=CARTESIAN_POINT('Ctrl Pts',(90.4430005297901,-3.84464515396214,1.54023198371691));
#15378=CARTESIAN_POINT('Ctrl Pts',(90.4430005297901,-3.89939440465314,1.42543769098813));
#15379=CARTESIAN_POINT('Ctrl Pts',(90.4430005297901,-3.9486855424696,1.30840674512748));
#15380=CARTESIAN_POINT('Ctrl Pts',(90.4430005297901,-3.99805880821873,1.19118080458689));
#15381=CARTESIAN_POINT('Ctrl Pts',(90.4430005297901,-4.04195599351763,1.07170998780389));
#15382=CARTESIAN_POINT('Ctrl Pts',(90.4430005297901,-4.08036631284025,0.950453612822061));
#15383=CARTESIAN_POINT('Ctrl Pts',(90.4430005297901,-4.11930037137882,0.82754386135488));
#15384=CARTESIAN_POINT('Ctrl Pts',(90.4430005297901,-4.15259726130455,0.70279877082149));
#15385=CARTESIAN_POINT('Ctrl Pts',(90.4430005297901,-4.18020045894591,0.576667891668107));
#15386=CARTESIAN_POINT('Ctrl Pts',(90.4430005297901,-4.20692512936151,0.454551381168132));
#15387=CARTESIAN_POINT('Ctrl Pts',(90.4430005297901,-4.22831276327775,0.331135046718066));
#15388=CARTESIAN_POINT('Ctrl Pts',(90.4430005297901,-4.24426791493629,0.206812112669407));
#15389=CARTESIAN_POINT('Ctrl Pts',(90.4430005297901,-4.24661469917407,0.188525912182953));
#15390=CARTESIAN_POINT('Ctrl Pts',(90.4430005297901,-4.24884387475333,0.170220083948822));
#15391=CARTESIAN_POINT('Ctrl Pts',(90.4430005297901,-4.25095505388501,0.151895867868624));
#15392=CARTESIAN_POINT('Ctrl Pts',(90.4430005297901,-4.25302188555424,0.133956570563175));
#15393=CARTESIAN_POINT('Ctrl Pts',(90.4430005297901,-4.25497512784511,0.116003677579542));
#15394=CARTESIAN_POINT('Ctrl Pts',(90.4430005297901,-4.25681383615621,0.0980463316274628));
#15395=CARTESIAN_POINT('Ctrl Pts',(90.4430005297901,-4.25874402274226,0.0791955829424464));
#15396=CARTESIAN_POINT('Ctrl Pts',(90.4430005297901,-4.2605482999999,0.0603373167362675));
#15397=CARTESIAN_POINT('Ctrl Pts',(90.4430005297901,-4.26222661848671,0.0414729768254311));
#15398=CARTESIAN_POINT('Ctrl Pts',(90.4430005297901,-4.27381294532833,-0.0887576138379506));
#15399=CARTESIAN_POINT('Ctrl Pts',(90.4430005297901,-4.27940028199616,-0.219276168214218));
#15400=CARTESIAN_POINT('Ctrl Pts',(90.4430005297901,-4.27910474674571,-0.349707946183935));
#15401=CARTESIAN_POINT('Ctrl Pts',(90.4430005297901,-4.27880600452057,-0.481555093074704));
#15402=CARTESIAN_POINT('Ctrl Pts',(90.4430005297901,-4.27249612571558,-0.613314293192436));
#15403=CARTESIAN_POINT('Ctrl Pts',(90.4430005297901,-4.26024353119921,-0.744611026846881));
#15404=CARTESIAN_POINT('Ctrl Pts',(90.4430005297901,-4.2544172843308,-0.807044104369089));
#15405=CARTESIAN_POINT('Ctrl Pts',(90.4430005297901,-4.24724656794793,-0.86937272698293));
#15406=CARTESIAN_POINT('Ctrl Pts',(90.4430005297901,-4.23873461501025,-0.931556866122166));
#15407=CARTESIAN_POINT('Ctrl Pts',(90.4430005297901,-4.2351230880836,-0.957940904492233));
#15408=CARTESIAN_POINT('Ctrl Pts',(90.4430005297901,-4.23126959330347,-0.984301416906842));
#15409=CARTESIAN_POINT('Ctrl Pts',(90.4430005297901,-4.22717812966965,-1.01061216318246));
#15410=CARTESIAN_POINT('Ctrl Pts',(90.4430005297901,-4.2065986047346,-1.14295176277282));
#15411=CARTESIAN_POINT('Ctrl Pts',(90.4430005297901,-4.17998717845608,-1.27415495149143));
#15412=CARTESIAN_POINT('Ctrl Pts',(90.4430005297901,-4.14743840998,-1.40383584303523));
#15413=CARTESIAN_POINT('Ctrl Pts',(90.4430005297901,-4.11495992051962,-1.53323672873422));
#15414=CARTESIAN_POINT('Ctrl Pts',(90.4430005297901,-4.07656968007687,-1.66112266026152));
#15415=CARTESIAN_POINT('Ctrl Pts',(90.4430005297901,-4.03231018308459,-1.78711174587462));
#15416=CARTESIAN_POINT('Ctrl Pts',(90.4430005297901,-4.00078732771841,-1.87684470701038));
#15417=CARTESIAN_POINT('Ctrl Pts',(90.4430005297901,-3.96628611272653,-1.96561551660628));
#15418=CARTESIAN_POINT('Ctrl Pts',(90.4430005297901,-3.92880598357856,-2.05328335682074));
#15419=CARTESIAN_POINT('Ctrl Pts',(90.4429666115571,0.0630101736086566,
3.72221671595325));
#15420=CARTESIAN_POINT('Ctrl Pts',(90.4434669596614,0.0519070659346713,
3.72240467081873));
#15421=CARTESIAN_POINT('Ctrl Pts',(90.4439673077658,0.0408031172722711,
3.72254294568215));
#15422=CARTESIAN_POINT('Ctrl Pts',(90.4444676558701,0.0296987722225578,
3.72263153500699));
#15423=CARTESIAN_POINT('Ctrl Pts',(82.4430005297902,1.9774016913413,3.97328893098977));
#15424=CARTESIAN_POINT('Ctrl Pts',(82.4430005297902,2.09010205945686,3.90686165204006));
#15425=CARTESIAN_POINT('Ctrl Pts',(82.4430005297901,2.19942886412691,3.83533535974096));
#15426=CARTESIAN_POINT('Ctrl Pts',(82.4430005297901,2.30496647500187,3.75870816478727));
#15427=CARTESIAN_POINT('Ctrl Pts',(82.4430005297901,2.31220701604366,3.75345105933093));
#15428=CARTESIAN_POINT('Ctrl Pts',(82.4430005297901,2.3194297087469,3.74816992928516));
#15429=CARTESIAN_POINT('Ctrl Pts',(82.4430005297901,2.32663441280681,3.74286476721896));
#15430=CARTESIAN_POINT('Ctrl Pts',(82.4430005297901,2.43426588168457,3.66361066030873));
#15431=CARTESIAN_POINT('Ctrl Pts',(82.4430005297901,2.53788621769259,3.57899596069104));
#15432=CARTESIAN_POINT('Ctrl Pts',(82.4430005297901,2.6373133241208,3.48943324204214));
#15433=CARTESIAN_POINT('Ctrl Pts',(82.4430005297901,2.71277582762782,3.4214575439359));
#15434=CARTESIAN_POINT('Ctrl Pts',(82.4430005297901,2.78582208230832,3.35063071617187));
#15435=CARTESIAN_POINT('Ctrl Pts',(82.4430005297901,2.85635530402485,3.27712288314481));
#15436=CARTESIAN_POINT('Ctrl Pts',(82.4430005297901,2.8718224849478,3.26100340178534));
#15437=CARTESIAN_POINT('Ctrl Pts',(82.4430005297901,2.88716274481628,3.2447612118818));
#15438=CARTESIAN_POINT('Ctrl Pts',(82.4430005297901,2.90237274291231,3.22840114134905));
#15439=CARTESIAN_POINT('Ctrl Pts',(82.4430005297901,2.99230521074578,3.13166861662084));
#15440=CARTESIAN_POINT('Ctrl Pts',(82.4430005297901,3.07771715585099,3.03078619899924));
#15441=CARTESIAN_POINT('Ctrl Pts',(82.4430005297901,3.158442407978,2.92616122334003));
#15442=CARTESIAN_POINT('Ctrl Pts',(82.4430005297901,3.23958388738415,2.82099679109442));
#15443=CARTESIAN_POINT('Ctrl Pts',(82.4430005297901,3.31599056878158,2.71205028395246));
#15444=CARTESIAN_POINT('Ctrl Pts',(82.4430005297901,3.38744699628565,2.59971212298357));
#15445=CARTESIAN_POINT('Ctrl Pts',(82.4430005297901,3.41263912973242,2.56010703718311));
#15446=CARTESIAN_POINT('Ctrl Pts',(82.4430005297901,3.43721553351162,2.52008024063316));
#15447=CARTESIAN_POINT('Ctrl Pts',(82.4430005297901,3.46116526677623,2.4796484520622));
#15448=CARTESIAN_POINT('Ctrl Pts',(82.4430005297901,3.47596320889566,2.45466665955338));
#15449=CARTESIAN_POINT('Ctrl Pts',(82.4430005297901,3.4905218915381,2.42953025043779));
#15450=CARTESIAN_POINT('Ctrl Pts',(82.4430005297901,3.50483857765273,2.4042431483245));
#15451=CARTESIAN_POINT('Ctrl Pts',(82.4430005297901,3.51750213823568,2.38187590865641));
#15452=CARTESIAN_POINT('Ctrl Pts',(82.4430005297901,3.52997604592585,2.35939102284286));
#15453=CARTESIAN_POINT('Ctrl Pts',(82.4430005297901,3.54224655904973,2.33681381979864));
#15454=CARTESIAN_POINT('Ctrl Pts',(82.4430005297901,3.60467283460315,2.22195222564727));
#15455=CARTESIAN_POINT('Ctrl Pts',(82.4430005297901,3.66192221873425,2.10455703827989));
#15456=CARTESIAN_POINT('Ctrl Pts',(82.4430005297901,3.71383452978784,1.98501482074639));
#15457=CARTESIAN_POINT('Ctrl Pts',(82.4430005297901,3.7654562526684,1.86614176152789));
#15458=CARTESIAN_POINT('Ctrl Pts',(82.4430005297901,3.81180071343808,1.74514481543744));
#15459=CARTESIAN_POINT('Ctrl Pts',(82.4430005297901,3.85266154558337,1.62238908638377));
#15460=CARTESIAN_POINT('Ctrl Pts',(82.4430005297901,3.8932624517446,1.50041423725836));
#15461=CARTESIAN_POINT('Ctrl Pts',(82.4430005297901,3.92844948626349,1.37670214001919));
#15462=CARTESIAN_POINT('Ctrl Pts',(82.4430005297901,3.95796854830322,1.25160798889632));
#15463=CARTESIAN_POINT('Ctrl Pts',(82.4430005297901,3.98748761034294,1.12651383777344));
#15464=CARTESIAN_POINT('Ctrl Pts',(82.4430005297901,4.0113389709295,1.00003688317767));
#15465=CARTESIAN_POINT('Ctrl Pts',(82.4430005297901,4.02921301288841,0.87254067379718));
#15466=CARTESIAN_POINT('Ctrl Pts',(82.4430005297901,4.03025722954012,0.865092237390291));
#15467=CARTESIAN_POINT('Ctrl Pts',(82.4430005297901,4.0312810292029,0.857640326545073));
#15468=CARTESIAN_POINT('Ctrl Pts',(82.4430005297901,4.03228434397425,0.850185015481216));
#15469=CARTESIAN_POINT('Ctrl Pts',(82.4430005297901,4.03459129039469,0.833042834718831));
#15470=CARTESIAN_POINT('Ctrl Pts',(82.4430005297901,4.03678865170643,0.815892170444972));
#15471=CARTESIAN_POINT('Ctrl Pts',(82.4430005297901,4.03887577431093,0.798735610694988));
#15472=CARTESIAN_POINT('Ctrl Pts',(82.4430005297901,4.05392301973012,0.675044283433661));
#15473=CARTESIAN_POINT('Ctrl Pts',(82.4430005297901,4.06324834973339,0.551017529415817));
#15474=CARTESIAN_POINT('Ctrl Pts',(82.4430005297901,4.06666460622852,0.426983323709972));
#15475=CARTESIAN_POINT('Ctrl Pts',(82.4430005297901,4.06939901272044,0.327705082224308));
#15476=CARTESIAN_POINT('Ctrl Pts',(82.4430005297901,4.06834683332202,0.228421806365612));
#15477=CARTESIAN_POINT('Ctrl Pts',(82.4430005297901,4.06338801735055,0.129303333680083));
#15478=CARTESIAN_POINT('Ctrl Pts',(82.4430005297901,4.05712876754241,0.00419135438749774));
#15479=CARTESIAN_POINT('Ctrl Pts',(82.4430005297901,4.04464633015305,-0.12065912809382));
#15480=CARTESIAN_POINT('Ctrl Pts',(82.4430005297901,4.02611519956499,-0.24482089419588));
#15481=CARTESIAN_POINT('Ctrl Pts',(82.4430005297901,4.00740439235759,-0.370186524588744));
#15482=CARTESIAN_POINT('Ctrl Pts',(82.4430005297901,3.98252663505701,-0.494850938703189));
#15483=CARTESIAN_POINT('Ctrl Pts',(82.4430005297901,3.9516152925171,-0.618346917085276));
#15484=CARTESIAN_POINT('Ctrl Pts',(82.4430005297901,3.94537341568365,-0.643284257981823));
#15485=CARTESIAN_POINT('Ctrl Pts',(82.4430005297901,3.93888539014275,-0.668173807600427));
#15486=CARTESIAN_POINT('Ctrl Pts',(82.4430005297901,3.93215207449842,-0.693011663701305));
#15487=CARTESIAN_POINT('Ctrl Pts',(82.4430005297901,3.92584560877593,-0.716274955724776));
#15488=CARTESIAN_POINT('Ctrl Pts',(82.4430005297901,3.91932525976329,-0.739487607266908));
#15489=CARTESIAN_POINT('Ctrl Pts',(82.4430005297901,3.91259863317221,-0.762624947309619));
#15490=CARTESIAN_POINT('Ctrl Pts',(82.4430005297901,3.87825099017711,-0.880769322485307));
#15491=CARTESIAN_POINT('Ctrl Pts',(82.4430005297901,3.83848575512177,-0.997112855082767));
#15492=CARTESIAN_POINT('Ctrl Pts',(82.4430005297901,3.79350625410374,-1.11126573136492));
#15493=CARTESIAN_POINT('Ctrl Pts',(82.4430005297901,3.74871960416427,-1.22492917346451));
#15494=CARTESIAN_POINT('Ctrl Pts',(82.4430005297901,3.6987628126906,-1.33642146078559));
#15495=CARTESIAN_POINT('Ctrl Pts',(82.4430005297901,3.64379183897507,-1.44533316841575));
#15496=CARTESIAN_POINT('Ctrl Pts',(82.4430005297901,3.59527253015452,-1.54146246028581));
#15497=CARTESIAN_POINT('Ctrl Pts',(82.4430005297901,3.54284611646389,-1.63558134564552));
#15498=CARTESIAN_POINT('Ctrl Pts',(82.4430005297901,3.48659512784046,-1.7273852613035));
#15499=CARTESIAN_POINT('Ctrl Pts',(82.4430005297901,3.4267302138798,-1.82508725102156));
#15500=CARTESIAN_POINT('Ctrl Pts',(82.4430005297901,3.36253323060098,-1.92016776201096));
#15501=CARTESIAN_POINT('Ctrl Pts',(82.4430005297901,3.2941636601901,-2.01234893030668));
#15502=CARTESIAN_POINT('Ctrl Pts',(82.4430005297901,3.28199925485566,-2.02874992695785));
#15503=CARTESIAN_POINT('Ctrl Pts',(82.4430005297901,3.26970271301345,-2.04505905011743));
#15504=CARTESIAN_POINT('Ctrl Pts',(82.4430005297901,3.25727487268007,-2.06127461217243));
#15505=CARTESIAN_POINT('Ctrl Pts',(82.4430005297901,3.2464949893423,-2.07533995760013));
#15506=CARTESIAN_POINT('Ctrl Pts',(82.4430005297901,3.23562112293147,-2.08932859706152));
#15507=CARTESIAN_POINT('Ctrl Pts',(82.4430005297901,3.22465780066579,-2.10323500148988));
#15508=CARTESIAN_POINT('Ctrl Pts',(82.4430005297901,3.15047393397067,-2.19733338036832));
#15509=CARTESIAN_POINT('Ctrl Pts',(82.4430005297901,3.07214423094984,-2.28773884704917));
#15510=CARTESIAN_POINT('Ctrl Pts',(82.4430005297901,2.98991394062545,-2.37420105585054));
#15511=CARTESIAN_POINT('Ctrl Pts',(82.4430005297901,2.90806315298578,-2.46026423115419));
#15512=CARTESIAN_POINT('Ctrl Pts',(82.4430005297901,2.82234707698341,-2.54242092978593));
#15513=CARTESIAN_POINT('Ctrl Pts',(82.4430005297901,2.73297569139553,-2.62038408613581));
#15514=CARTESIAN_POINT('Ctrl Pts',(82.4430005297901,2.64463815610224,-2.69744536285576));
#15515=CARTESIAN_POINT('Ctrl Pts',(82.4430005297901,2.55272879796832,-2.77040993931852));
#15516=CARTESIAN_POINT('Ctrl Pts',(82.4430005297901,2.45742821329426,-2.83895504478));
#15517=CARTESIAN_POINT('Ctrl Pts',(82.4430005297901,2.3621276286202,-2.90750015024147));
#15518=CARTESIAN_POINT('Ctrl Pts',(82.4430005297901,2.26343528681409,-2.97162624539));
#15519=CARTESIAN_POINT('Ctrl Pts',(82.4430005297901,2.16151778945158,-3.03095833168065));
#15520=CARTESIAN_POINT('Origin',(81.4430005297901,0.,0.));
#15521=CARTESIAN_POINT('',(82.4430005297901,-5.42440960677665,-6.64298586220318E-16));
#15522=CARTESIAN_POINT('Origin',(82.4430005297901,0.,0.));
#15523=CARTESIAN_POINT('',(81.4430005297901,-5.42440960677665,-6.64298586220318E-16));
#15524=CARTESIAN_POINT('',(81.4430005297901,-5.42440960677665,-6.64298586220318E-16));
#15525=CARTESIAN_POINT('Origin',(81.4430005297901,0.,0.));
#15526=CARTESIAN_POINT('Origin',(82.4430005297901,0.,0.));
#15527=CARTESIAN_POINT('Origin',(90.4430005297901,0.,0.));
#15528=CARTESIAN_POINT('Origin',(81.4430005297901,0.,0.));
#15529=CARTESIAN_POINT('',(0.,0.,0.));
#15530=CARTESIAN_POINT('Origin',(66.9886855842388,0.,0.));
#15531=CARTESIAN_POINT('',(66.7386855842388,-9.21957102532866E-16,7.52835105742136));
#15532=CARTESIAN_POINT('Origin',(66.7386855842388,0.,0.));
#15533=CARTESIAN_POINT('',(67.2386855842388,8.60724762575498E-16,7.02835105742136));
#15534=CARTESIAN_POINT('',(66.9886855842388,8.91340932554182E-16,7.27835105742136));
#15535=CARTESIAN_POINT('Origin',(67.2386855842388,0.,0.));
#15536=CARTESIAN_POINT('Origin',(67.2386855842388,0.,-8.84759007750164));
#15537=CARTESIAN_POINT('',(67.2386855842388,-7.86249045812787E-16,6.42021067919505));
#15538=CARTESIAN_POINT('Origin',(67.2386855842388,0.,0.));
#15539=CARTESIAN_POINT('Origin',(48.2427605064424,0.,0.));
#15540=CARTESIAN_POINT('',(21.6431770351805,-9.21957102532866E-16,7.52835105742136));
#15541=CARTESIAN_POINT('',(48.2427605064424,-9.21957102532866E-16,7.52835105742136));
#15542=CARTESIAN_POINT('Origin',(21.6431770351805,0.,0.));
#15543=CARTESIAN_POINT('Origin',(15.8714473032184,0.,0.));
#15544=CARTESIAN_POINT('',(15.8714473032184,3.29760625124175,0.999999999999998));
#15545=CARTESIAN_POINT('',(14.8714473032184,3.44589712386029,-6.01983033610089E-17));
#15546=CARTESIAN_POINT('Ctrl Pts',(15.8714473032184,3.29760625124174,0.999999999999999));
#15547=CARTESIAN_POINT('Ctrl Pts',(15.9978139569531,3.29760625124174,0.999999999999999));
#15548=CARTESIAN_POINT('Ctrl Pts',(16.132068844028,3.30562953237115,0.974596096350375));
#15549=CARTESIAN_POINT('Ctrl Pts',(16.3782103010389,3.33407731229027,0.872325929581351));
#15550=CARTESIAN_POINT('Ctrl Pts',(16.4901654582252,3.3540348875684,0.795495407366277));
#15551=CARTESIAN_POINT('Ctrl Pts',(16.6669197871454,3.39109395594973,0.618741078446085));
#15552=CARTESIAN_POINT('Ctrl Pts',(16.7437680872924,3.41067812574963,0.506776556958312));
#15553=CARTESIAN_POINT('Ctrl Pts',(16.8460513462857,3.43826042485992,0.26060123975522));
#15554=CARTESIAN_POINT('Ctrl Pts',(16.8714473032184,3.44589712386029,0.126333880758864));
#15555=CARTESIAN_POINT('Ctrl Pts',(16.8714473032184,3.44589712386029,-0.126333880758864));
#15556=CARTESIAN_POINT('Ctrl Pts',(16.8460513462857,3.43826042485992,-0.260601239755222));
#15557=CARTESIAN_POINT('Ctrl Pts',(16.7437680872924,3.41067812574963,-0.506776556958312));
#15558=CARTESIAN_POINT('Ctrl Pts',(16.6669197871454,3.39109395594973,-0.618741078446085));
#15559=CARTESIAN_POINT('Ctrl Pts',(16.4901654582252,3.3540348875684,-0.795495407366277));
#15560=CARTESIAN_POINT('Ctrl Pts',(16.3782103010389,3.33407731229027,-0.872325929581349));
#15561=CARTESIAN_POINT('Ctrl Pts',(16.132068844028,3.30562953237115,-0.974596096350375));
#15562=CARTESIAN_POINT('Ctrl Pts',(15.9978139569531,3.29760625124174,-0.999999999999999));
#15563=CARTESIAN_POINT('Ctrl Pts',(15.7450806494837,3.29760625124174,-0.999999999999999));
#15564=CARTESIAN_POINT('Ctrl Pts',(15.6108257624088,3.30562953237115,-0.974596096350376));
#15565=CARTESIAN_POINT('Ctrl Pts',(15.3646843053979,3.33407731229027,-0.872325929581351));
#15566=CARTESIAN_POINT('Ctrl Pts',(15.2527291482116,3.3540348875684,-0.795495407366277));
#15567=CARTESIAN_POINT('Ctrl Pts',(15.0759748192914,3.39109395594973,-0.618741078446085));
#15568=CARTESIAN_POINT('Ctrl Pts',(14.9991265191444,3.41067812574963,-0.506776556958314));
#15569=CARTESIAN_POINT('Ctrl Pts',(14.8968432601511,3.43826042485992,-0.260601239755224));
#15570=CARTESIAN_POINT('Ctrl Pts',(14.8714473032184,3.44589712386029,-0.126333880758864));
#15571=CARTESIAN_POINT('Ctrl Pts',(14.8714473032184,3.44589712386029,-2.42861286636753E-16));
#15572=CARTESIAN_POINT('Ctrl Pts',(14.8714473032184,3.44589712386029,-1.38777878078145E-16));
#15573=CARTESIAN_POINT('Ctrl Pts',(14.8714473032184,3.44589712386029,0.126333880758864));
#15574=CARTESIAN_POINT('Ctrl Pts',(14.8968432601511,3.43826042485992,0.260601239755221));
#15575=CARTESIAN_POINT('Ctrl Pts',(14.9991265191444,3.41067812574963,0.506776556958312));
#15576=CARTESIAN_POINT('Ctrl Pts',(15.0759748192914,3.39109395594973,0.618741078446085));
#15577=CARTESIAN_POINT('Ctrl Pts',(15.2527291482116,3.3540348875684,0.795495407366277));
#15578=CARTESIAN_POINT('Ctrl Pts',(15.3646843053979,3.33407731229027,0.872325929581349));
#15579=CARTESIAN_POINT('Ctrl Pts',(15.6108257624088,3.30562953237115,0.974596096350375));
#15580=CARTESIAN_POINT('Ctrl Pts',(15.7450806494837,3.29760625124174,0.999999999999999));
#15581=CARTESIAN_POINT('Ctrl Pts',(15.8714473032184,3.29760625124174,0.999999999999999));
#15582=CARTESIAN_POINT('',(14.8714473032184,7.52312685038423,1.22464679914735E-16));
#15583=CARTESIAN_POINT('',(14.8714473032184,0.,1.22464679914735E-16));
#15584=CARTESIAN_POINT('',(15.8714473032184,7.45636892910833,0.999999999999999));
#15585=CARTESIAN_POINT('Ctrl Pts',(15.8714473032184,7.45636892910833,0.999999999999999));
#15586=CARTESIAN_POINT('Ctrl Pts',(15.7457245010652,7.45636892910833,0.999999999999999));
#15587=CARTESIAN_POINT('Ctrl Pts',(15.6117245964979,7.45987689127736,0.974843764196788));
#15588=CARTESIAN_POINT('Ctrl Pts',(15.3653900481838,7.47250970222183,0.872744136330349));
#15589=CARTESIAN_POINT('Ctrl Pts',(15.2530425360435,7.48144799782428,0.795808795198177));
#15590=CARTESIAN_POINT('Ctrl Pts',(15.0756394573932,7.49819644864561,0.618405716547907));
#15591=CARTESIAN_POINT('Ctrl Pts',(14.9987033720303,7.50710016352641,0.506057792670463));
#15592=CARTESIAN_POINT('Ctrl Pts',(14.8966032000273,7.51965370990447,0.259721846141313));
#15593=CARTESIAN_POINT('Ctrl Pts',(14.8714473032184,7.52312685038423,0.125721456548635));
#15594=CARTESIAN_POINT('Ctrl Pts',(14.8714473032184,7.52312685038423,-1.04083408558608E-16));
#15595=CARTESIAN_POINT('Ctrl Pts',(14.8714473032184,7.52312685038423,-2.08166817117217E-16));
#15596=CARTESIAN_POINT('Ctrl Pts',(14.8714473032184,7.52312685038423,-0.125721456548636));
#15597=CARTESIAN_POINT('Ctrl Pts',(14.8966032000273,7.51965370990447,-0.259721846141313));
#15598=CARTESIAN_POINT('Ctrl Pts',(14.9987033720303,7.50710016352641,-0.506057792670463));
#15599=CARTESIAN_POINT('Ctrl Pts',(15.0756394573932,7.49819644864561,-0.618405716547907));
#15600=CARTESIAN_POINT('Ctrl Pts',(15.2530425360435,7.48144799782428,-0.795808795198177));
#15601=CARTESIAN_POINT('Ctrl Pts',(15.3653900481838,7.47250970222183,-0.872744136330348));
#15602=CARTESIAN_POINT('Ctrl Pts',(15.6117245964979,7.45987689127736,-0.974843764196788));
#15603=CARTESIAN_POINT('Ctrl Pts',(15.7457245010652,7.45636892910833,-0.999999999999999));
#15604=CARTESIAN_POINT('Ctrl Pts',(15.9971701053716,7.45636892910833,-0.999999999999999));
#15605=CARTESIAN_POINT('Ctrl Pts',(16.1311700099389,7.45987689127736,-0.974843764196788));
#15606=CARTESIAN_POINT('Ctrl Pts',(16.377504558253,7.47250970222183,-0.872744136330349));
#15607=CARTESIAN_POINT('Ctrl Pts',(16.4898520703933,7.48144799782428,-0.795808795198177));
#15608=CARTESIAN_POINT('Ctrl Pts',(16.6672551490436,7.49819644864561,-0.618405716547907));
#15609=CARTESIAN_POINT('Ctrl Pts',(16.7441912344065,7.50710016352641,-0.506057792670463));
#15610=CARTESIAN_POINT('Ctrl Pts',(16.8462914064095,7.51965370990447,-0.259721846141313));
#15611=CARTESIAN_POINT('Ctrl Pts',(16.8714473032184,7.52312685038423,-0.125721456548635));
#15612=CARTESIAN_POINT('Ctrl Pts',(16.8714473032184,7.52312685038423,0.125721456548635));
#15613=CARTESIAN_POINT('Ctrl Pts',(16.8462914064095,7.51965370990447,0.259721846141313));
#15614=CARTESIAN_POINT('Ctrl Pts',(16.7441912344065,7.50710016352641,0.506057792670463));
#15615=CARTESIAN_POINT('Ctrl Pts',(16.6672551490436,7.49819644864561,0.618405716547907));
#15616=CARTESIAN_POINT('Ctrl Pts',(16.4898520703933,7.48144799782428,0.795808795198176));
#15617=CARTESIAN_POINT('Ctrl Pts',(16.377504558253,7.47250970222183,0.872744136330349));
#15618=CARTESIAN_POINT('Ctrl Pts',(16.1311700099389,7.45987689127736,0.974843764196788));
#15619=CARTESIAN_POINT('Ctrl Pts',(15.9971701053716,7.45636892910833,0.999999999999999));
#15620=CARTESIAN_POINT('Ctrl Pts',(15.8714473032184,7.45636892910833,0.999999999999999));
#15621=CARTESIAN_POINT('Origin',(11.0238490761438,0.,0.));
#15622=CARTESIAN_POINT('',(11.0238490761438,5.,-6.12323399573677E-16));
#15623=CARTESIAN_POINT('Origin',(11.0238490761438,0.,0.));
#15624=CARTESIAN_POINT('',(12.0767011645438,5.,-6.12323399573677E-16));
#15625=CARTESIAN_POINT('',(11.0238490761438,5.,6.12323399573677E-16));
#15626=CARTESIAN_POINT('Origin',(12.0767011645438,0.,0.));
#15627=CARTESIAN_POINT('Origin',(12.0767011645438,0.,0.));
#15628=CARTESIAN_POINT('',(12.076701164516,-4.22000688292658E-16,3.44589712386029));
#15629=CARTESIAN_POINT('Origin',(12.076701164516,0.,0.));
#15630=CARTESIAN_POINT('Origin',(11.474739121518,0.,0.));
#15631=CARTESIAN_POINT('',(11.9256291668923,-9.21317321690256E-16,7.52312685038423));
#15632=CARTESIAN_POINT('Origin',(11.9256291668923,0.,0.));
#15633=CARTESIAN_POINT('',(11.0238490761438,-8.44001376585316E-16,6.89179424772059));
#15634=CARTESIAN_POINT('',(11.474739121518,-8.82659349137786E-16,7.20746054905241));
#15635=CARTESIAN_POINT('Origin',(11.0238490761438,0.,0.));
#15636=CARTESIAN_POINT('Origin',(16.3019119808107,0.,0.));
#15637=CARTESIAN_POINT('',(20.6781947947292,-9.21317321690256E-16,7.52312685038423));
#15638=CARTESIAN_POINT('Origin',(20.6781947947292,0.,0.));
#15639=CARTESIAN_POINT('',(16.3019119808107,-9.21317321690256E-16,7.52312685038423));
#15640=CARTESIAN_POINT('Origin',(20.9315098273138,0.,0.));
#15641=CARTESIAN_POINT('',(21.1848248598985,-8.82659349137786E-16,7.20746054905241));
#15642=CARTESIAN_POINT('',(20.9315098273138,9.01988335414021E-16,7.36529369971832));
#15643=CARTESIAN_POINT('Origin',(21.1848248598985,0.,0.));
#15644=CARTESIAN_POINT('Origin',(21.4140009475395,0.,0.));
#15645=CARTESIAN_POINT('',(21.4140009475395,-9.02308225835327E-16,7.36790580323689));
#15646=CARTESIAN_POINT('Origin',(53.9616500647475,0.,0.));
#15647=CARTESIAN_POINT('',(31.6525499953511,-7.84960767273423E-16,6.40969108660508));
#15648=CARTESIAN_POINT('Origin',(31.6525499953511,0.,0.));
#15649=CARTESIAN_POINT('',(53.9616500647475,-7.85768394580416E-16,6.41628586403442));
#15650=CARTESIAN_POINT('Origin',(31.0318089645314,0.,0.));
#15651=CARTESIAN_POINT('',(30.4110679337117,-7.84960767273423E-16,6.40969108660508));
#15652=CARTESIAN_POINT('Origin',(30.4110679337117,0.,0.));
#15653=CARTESIAN_POINT('',(31.0318089645314,-7.84960767273423E-16,6.40969108660508));
#15654=CARTESIAN_POINT('Origin',(29.5420239984498,0.,0.));
#15655=CARTESIAN_POINT('',(28.6729800631879,-7.84852901782084E-16,6.40881029802658));
#15656=CARTESIAN_POINT('Origin',(28.6729800631879,0.,0.));
#15657=CARTESIAN_POINT('',(29.5420239984498,-7.84884362648318E-16,6.40906719549494));
#15658=CARTESIAN_POINT('Origin',(28.6729800631879,0.,-6.41550316824698));
#15659=CARTESIAN_POINT('',(28.6729800631879,-7.85672541991337E-16,6.41550316824698));
#15660=CARTESIAN_POINT('Origin',(28.6729800631879,0.,0.));
#15661=CARTESIAN_POINT('Origin',(28.2136282688352,0.,0.));
#15662=CARTESIAN_POINT('',(27.7542764744824,-7.85672541991337E-16,6.41550316824698));
#15663=CARTESIAN_POINT('Origin',(27.7542764744824,0.,0.));
#15664=CARTESIAN_POINT('',(28.2136282688352,-7.85672541991337E-16,6.41550316824698));
#15665=CARTESIAN_POINT('Origin',(27.7542764744824,0.,-6.40853872070288));
#15666=CARTESIAN_POINT('',(27.7542764744824,-7.84819643152065E-16,6.40853872070288));
#15667=CARTESIAN_POINT('Origin',(27.7542764744824,0.,0.));
#15668=CARTESIAN_POINT('Origin',(26.6245076505395,0.,0.));
#15669=CARTESIAN_POINT('',(25.4947388265965,-7.84737844052149E-16,6.40787078036307));
#15670=CARTESIAN_POINT('Origin',(25.4947388265965,0.,0.));
#15671=CARTESIAN_POINT('',(26.6245076505395,-7.84778743602106E-16,6.40820475053297));
#15672=CARTESIAN_POINT('Origin',(25.0105689136245,0.,0.));
#15673=CARTESIAN_POINT('',(24.5263990006525,-7.84737844052149E-16,6.40787078036307));
#15674=CARTESIAN_POINT('Origin',(24.5263990006525,0.,0.));
#15675=CARTESIAN_POINT('',(25.0105689136245,-7.84737844052149E-16,6.40787078036307));
#15676=CARTESIAN_POINT('Origin',(23.6497386319918,0.,0.));
#15677=CARTESIAN_POINT('',(22.7730782633312,-7.84639315317936E-16,6.40706623219228));
#15678=CARTESIAN_POINT('Origin',(22.7730782633312,0.,0.));
#15679=CARTESIAN_POINT('',(23.6497386319918,-7.84671051911994E-16,6.40732538114918));
#15680=CARTESIAN_POINT('Origin',(22.2310089528171,0.,0.));
#15681=CARTESIAN_POINT('',(21.688939642303,-7.84639315317937E-16,6.40706623219228));
#15682=CARTESIAN_POINT('Origin',(21.688939642303,0.,0.));
#15683=CARTESIAN_POINT('',(22.2310089528171,-7.84639315317937E-16,6.40706623219228));
#15684=CARTESIAN_POINT('Origin',(21.4368822511007,0.,0.));
#15685=CARTESIAN_POINT('',(21.1848248598985,-7.8458181784762E-16,6.4065967297173));
#15686=CARTESIAN_POINT('Origin',(21.1848248598985,0.,0.));
#15687=CARTESIAN_POINT('',(21.4368822511007,-7.84590942753216E-16,6.40667124022599));
#15688=CARTESIAN_POINT('Origin',(21.1848248598985,0.,-4.66385643997278));
#15689=CARTESIAN_POINT('',(21.1848248598985,-5.71157686089543E-16,4.66385643997278));
#15690=CARTESIAN_POINT('Origin',(21.1848248598985,0.,0.));
#15691=CARTESIAN_POINT('Origin',(20.4983944566926,0.,0.));
#15692=CARTESIAN_POINT('',(19.8119640534868,-5.71157686089543E-16,4.66385643997278));
#15693=CARTESIAN_POINT('Origin',(19.8119640534868,0.,0.));
#15694=CARTESIAN_POINT('',(20.4983944566926,-5.71157686089543E-16,4.66385643997278));
#15695=CARTESIAN_POINT('Origin',(19.8119640534868,0.,-3.44589712386029));
#15696=CARTESIAN_POINT('',(19.8119640534868,-4.22000688292658E-16,3.44589712386029));
#15697=CARTESIAN_POINT('Origin',(19.8119640534868,0.,0.));
#15698=CARTESIAN_POINT('Origin',(15.9443326090014,0.,0.));
#15699=CARTESIAN_POINT('',(15.9443326090014,-4.22000688292657E-16,3.44589712386029));
#15700=CARTESIAN_POINT('Origin',(11.0238490761438,0.,-6.89179424772059));
#15701=CARTESIAN_POINT('',(0.,0.,0.));
#15702=CARTESIAN_POINT('Origin',(30.1110679337117,0.,0.));
#15703=CARTESIAN_POINT('',(30.4110679337117,-7.4816555742545E-16,6.10923539706593));
#15704=CARTESIAN_POINT('Origin',(30.4110679337117,0.,0.));
#15705=CARTESIAN_POINT('',(30.1109792509259,-7.84904959794637E-16,6.4092353839582));
#15706=CARTESIAN_POINT('Origin',(30.1110679337117,-7.4816555742545E-16,
6.10923539706593));
#15707=CARTESIAN_POINT('Origin',(30.1109792509259,-7.84904959794637E-16,
0.));
#15708=CARTESIAN_POINT('Origin',(29.5420239984498,0.,0.));
#15709=CARTESIAN_POINT('',(28.9728913804021,-7.84863759081066E-16,6.40889895460077));
#15710=CARTESIAN_POINT('',(29.5420239984498,-7.84884362648318E-16,6.40906719549494));
#15711=CARTESIAN_POINT('Origin',(28.9728913804021,-7.84863759081066E-16,
0.));
#15712=CARTESIAN_POINT('Origin',(30.4110679337117,0.,0.));
#15713=CARTESIAN_POINT('Origin',(28.9729800631879,0.,0.));
#15714=CARTESIAN_POINT('',(28.6729800631879,-7.48124356711879E-16,6.1088989677085));
#15715=CARTESIAN_POINT('Origin',(28.9729800631879,-7.48124356711878E-16,
6.1088989677085));
#15716=CARTESIAN_POINT('Origin',(28.6729800631879,0.,0.));
#15717=CARTESIAN_POINT('Origin',(28.6729800631879,0.,-6.40881029802658));
#15718=CARTESIAN_POINT('',(0.,0.,0.));
#15719=CARTESIAN_POINT('Origin',(66.9212607628943,0.,0.));
#15720=CARTESIAN_POINT('',(90.7335918111184,-2.00577712042713E-11,2.204));
#15721=CARTESIAN_POINT('',(90.6260478258334,0.0018616288768175,2.20399921377888));
#15722=CARTESIAN_POINT('',(66.9212607628943,-2.69912154532077E-16,2.204));
#15723=CARTESIAN_POINT('',(90.7336894293003,0.00186538422401548,2.20367257219299));
#15724=CARTESIAN_POINT('Ctrl Pts',(90.7335918111184,-2.00577712042713E-11,
2.204));
#15725=CARTESIAN_POINT('Ctrl Pts',(90.733561597852,0.000618820167389943,
2.20400000000001));
#15726=CARTESIAN_POINT('Ctrl Pts',(90.7335313878983,0.00123764367719169,
2.20399973937949));
#15727=CARTESIAN_POINT('Ctrl Pts',(90.7335011812186,0.0018564703451418,
2.20399921813005));
#15728=CARTESIAN_POINT('',(90.3514582376541,-0.174123623218802,-2.19796285666152));
#15729=CARTESIAN_POINT('Ctrl Pts',(90.7336894293003,0.00186538422401548,
2.20367257219299));
#15730=CARTESIAN_POINT('Ctrl Pts',(90.7297945009894,0.0795614518465619,
2.20378293938922));
#15731=CARTESIAN_POINT('Ctrl Pts',(90.7259488838733,0.157101568214134,2.19980889002447));
#15732=CARTESIAN_POINT('Ctrl Pts',(90.7220854782314,0.234095693825053,2.19178159250512));
#15733=CARTESIAN_POINT('Ctrl Pts',(90.7214381250115,0.246996848855024,2.19043653651615));
#15734=CARTESIAN_POINT('Ctrl Pts',(90.7207902723531,0.259882780727669,2.18897762717947));
#15735=CARTESIAN_POINT('Ctrl Pts',(90.720141604586,0.272751779700561,2.18740494157558));
#15736=CARTESIAN_POINT('Ctrl Pts',(90.7164410672004,0.346167192379334,2.1784330422952));
#15737=CARTESIAN_POINT('Ctrl Pts',(90.7127132590446,0.419029635902584,2.16575942048269));
#15738=CARTESIAN_POINT('Ctrl Pts',(90.7088849599204,0.490986234289347,2.14943329737029));
#15739=CARTESIAN_POINT('Ctrl Pts',(90.7079697249612,0.508188963819403,2.14553019624443));
#15740=CARTESIAN_POINT('Ctrl Pts',(90.7070487464506,0.525340152219468,2.14141830628492));
#15741=CARTESIAN_POINT('Ctrl Pts',(90.7061210239026,0.542435412378799,2.13709822000947));
#15742=CARTESIAN_POINT('Ctrl Pts',(90.7042020379602,0.577796807870508,2.12816215949207));
#15743=CARTESIAN_POINT('Ctrl Pts',(90.7022539890451,0.612917098866179,2.11833617853689));
#15744=CARTESIAN_POINT('Ctrl Pts',(90.7002675857539,0.647753314711685,2.10762898576747));
#15745=CARTESIAN_POINT('Ctrl Pts',(90.7002659993789,0.647781135499218,2.10762043482334));
#15746=CARTESIAN_POINT('Ctrl Pts',(90.7002644129794,0.647808956105774,2.10761188331721));
#15747=CARTESIAN_POINT('Ctrl Pts',(90.7002628265554,0.647836776531331,2.10760333124909));
#15748=CARTESIAN_POINT('Ctrl Pts',(90.6965577230164,0.712811561377226,2.08762992053154));
#15749=CARTESIAN_POINT('Ctrl Pts',(90.6927132629296,0.776943472303309,2.0645398564198));
#15750=CARTESIAN_POINT('Ctrl Pts',(90.6887955534437,0.839929315709657,2.03845326069095));
#15751=CARTESIAN_POINT('Ctrl Pts',(90.6884085760281,0.846150833407494,2.03587651950235));
#15752=CARTESIAN_POINT('Ctrl Pts',(90.6880208839337,0.852361146062634,2.03327057681406));
#15753=CARTESIAN_POINT('Ctrl Pts',(90.6876325408708,0.858559946859202,2.03063557170245));
#15754=CARTESIAN_POINT('Ctrl Pts',(90.6833190288938,0.927412989524639,2.00136731073919));
#15755=CARTESIAN_POINT('Ctrl Pts',(90.6789258022943,0.994849372636953,1.96850876260346));
#15756=CARTESIAN_POINT('Ctrl Pts',(90.6745280179299,1.06049739929679,1.93225792133409));
#15757=CARTESIAN_POINT('Ctrl Pts',(90.6701353803395,1.12606859737061,1.89604950481102));
#15758=CARTESIAN_POINT('Ctrl Pts',(90.6657385446255,1.18985584872898,1.85645702888921));
#15759=CARTESIAN_POINT('Ctrl Pts',(90.6613932375148,1.2515156647503,1.8137078109801));
#15760=CARTESIAN_POINT('Ctrl Pts',(90.6570506864659,1.3131363723121,1.77098570726246));
#15761=CARTESIAN_POINT('Ctrl Pts',(90.6527597693697,1.37263246530918,1.72511099080974));
#15762=CARTESIAN_POINT('Ctrl Pts',(90.6485531215493,1.42968534561502,1.67633745923008));
#15763=CARTESIAN_POINT('Ctrl Pts',(90.6443477744083,1.48672058538981,1.62757900823869));
#15764=CARTESIAN_POINT('Ctrl Pts',(90.6402329784846,1.5413063978217,1.57591591928549));
#15765=CARTESIAN_POINT('Ctrl Pts',(90.6362010534082,1.59316699803034,1.52164672579692));
#15766=CARTESIAN_POINT('Ctrl Pts',(90.632169064372,1.64502842092154,1.46737667141745));
#15767=CARTESIAN_POINT('Ctrl Pts',(90.6282324700559,1.6941492376414,1.41048483893202));
#15768=CARTESIAN_POINT('Ctrl Pts',(90.6243716777576,1.74026179806897,1.35128061019675));
#15769=CARTESIAN_POINT('Ctrl Pts',(90.6205068779001,1.78642222401146,1.2920149266026));
#15770=CARTESIAN_POINT('Ctrl Pts',(90.6167178746548,1.82956807036417,1.23043181827767));
#15771=CARTESIAN_POINT('Ctrl Pts',(90.6129652394984,1.8694534254963,1.16686432476613));
#15772=CARTESIAN_POINT('Ctrl Pts',(90.6092106191631,1.90935988035278,1.10326320345846));
#15773=CARTESIAN_POINT('Ctrl Pts',(90.6054920937299,1.94600205189049,1.03767547158359));
#15774=CARTESIAN_POINT('Ctrl Pts',(90.6017507504073,1.97916382080471,0.970463227410216));
#15775=CARTESIAN_POINT('Ctrl Pts',(90.5980026321539,2.01238563999263,0.903129273394721));
#15776=CARTESIAN_POINT('Ctrl Pts',(90.5942311045093,2.0421138920473,0.834164813775563));
#15777=CARTESIAN_POINT('Ctrl Pts',(90.5903635513674,2.06816820064445,0.763964378509355));
#15778=CARTESIAN_POINT('Ctrl Pts',(90.5873426674423,2.08851880453662,0.709131940878822));
#15779=CARTESIAN_POINT('Ctrl Pts',(90.5842627906181,2.10662855118927,0.653546080199383));
#15780=CARTESIAN_POINT('Ctrl Pts',(90.5810873112824,2.12243098826343,0.597407926020108));
#15781=CARTESIAN_POINT('Ctrl Pts',(90.5810857578706,2.12243871865304,0.597380463812735));
#15782=CARTESIAN_POINT('Ctrl Pts',(90.5810842044359,2.12244644849101,0.597353001472851));
#15783=CARTESIAN_POINT('Ctrl Pts',(90.5810826509783,2.12245417777735,0.597325539000468));
#15784=CARTESIAN_POINT('Ctrl Pts',(90.5773740556272,2.14090643281885,0.53176391766318));
#15785=CARTESIAN_POINT('Ctrl Pts',(90.5735258965146,2.15626954801148,0.465221864236195));
#15786=CARTESIAN_POINT('Ctrl Pts',(90.5696041138388,2.16848067480506,0.398020314951632));
#15787=CARTESIAN_POINT('Ctrl Pts',(90.5692131468832,2.16969801586171,0.391320916411502));
#15788=CARTESIAN_POINT('Ctrl Pts',(90.568821448233,2.17088404874851,0.384615002656172));
#15789=CARTESIAN_POINT('Ctrl Pts',(90.5684290832191,2.17203872326328,0.377902917265477));
#15790=CARTESIAN_POINT('Ctrl Pts',(90.5641072789612,2.18475717944205,0.30397094525284));
#15791=CARTESIAN_POINT('Ctrl Pts',(90.5597052322467,2.1936691058592,0.229284601525099));
#15792=CARTESIAN_POINT('Ctrl Pts',(90.5552981347378,2.19874006138384,0.154265805746006));
#15793=CARTESIAN_POINT('Ctrl Pts',(90.5508962519783,2.20380501664133,0.0793357768302387));
#15794=CARTESIAN_POINT('Ctrl Pts',(90.5464896818778,2.20503846321057,0.0040740489741147));
#15795=CARTESIAN_POINT('Ctrl Pts',(90.5421341666814,2.20244590853611,-0.0711054635678189));
#15796=CARTESIAN_POINT('Ctrl Pts',(90.5377814559523,2.19985502317853,-0.146236568865197));
#15797=CARTESIAN_POINT('Ctrl Pts',(90.5334799059467,2.19344323608003,-0.221285605287203));
#15798=CARTESIAN_POINT('Ctrl Pts',(90.5292621250607,2.18325177058937,-0.295845329434535));
#15799=CARTESIAN_POINT('Ctrl Pts',(90.52504570996,2.17306360525912,-0.370380909944266));
#15800=CARTESIAN_POINT('Ctrl Pts',(90.520915988809,2.15909328609742,-0.444426385491838));
#15801=CARTESIAN_POINT('Ctrl Pts',(90.5168735963798,2.14142863128311,-0.517583194118507));
#15802=CARTESIAN_POINT('Ctrl Pts',(90.5128312191312,2.12376404280608,-0.590739728014407));
#15803=CARTESIAN_POINT('Ctrl Pts',(90.5088819801313,2.10239512026904,-0.663005499997299));
#15804=CARTESIAN_POINT('Ctrl Pts',(90.5050078670583,2.07743449591428,-0.733985551508349));
#15805=CARTESIAN_POINT('Ctrl Pts',(90.5011299379722,2.05244928526926,-0.805035518584183));
#15806=CARTESIAN_POINT('Ctrl Pts',(90.4973271166733,2.02386508098874,-0.874797196413565));
#15807=CARTESIAN_POINT('Ctrl Pts',(90.4935598951022,1.99182912744931,-0.942881395836193));
#15808=CARTESIAN_POINT('Ctrl Pts',(90.4897907742079,1.95977702231683,-1.01099992132566));
#15809=CARTESIAN_POINT('Ctrl Pts',(90.486056972178,1.92426938925078,-1.0774390560734));
#15810=CARTESIAN_POINT('Ctrl Pts',(90.4822995779161,1.88549419873164,-1.14181879687684));
#15811=CARTESIAN_POINT('Ctrl Pts',(90.4785356605338,1.84665169155259,-1.20631030577369));
#15812=CARTESIAN_POINT('Ctrl Pts',(90.4747475531196,1.80452988119458,-1.26873485386227));
#15813=CARTESIAN_POINT('Ctrl Pts',(90.4708628272517,1.75936358523186,-1.32872489694982));
#15814=CARTESIAN_POINT('Ctrl Pts',(90.4679364284152,1.72533940940893,-1.37391593442875));
#15815=CARTESIAN_POINT('Ctrl Pts',(90.4649548266515,1.68958847284266,-1.41772564327571));
#15816=CARTESIAN_POINT('Ctrl Pts',(90.4618853553014,1.65223033111774,-1.46000507888003));
#15817=CARTESIAN_POINT('Ctrl Pts',(90.4618838551247,1.65221207265925,-1.460025742577));
#15818=CARTESIAN_POINT('Ctrl Pts',(90.4618823549269,1.65219381381683,-1.46004640590898));
#15819=CARTESIAN_POINT('Ctrl Pts',(90.4618808547082,1.65217555459052,-1.46006706887596));
#15820=CARTESIAN_POINT('Ctrl Pts',(90.4581925626705,1.60728519424155,-1.51086703256677));
#15821=CARTESIAN_POINT('Ctrl Pts',(90.454368077417,1.55991156807906,-1.55963231878916));
#15822=CARTESIAN_POINT('Ctrl Pts',(90.4504725371015,1.51028778213619,-1.60613397507167));
#15823=CARTESIAN_POINT('Ctrl Pts',(90.4501137585467,1.50571744047351,-1.6104167691603));
#15824=CARTESIAN_POINT('Ctrl Pts',(90.4497543772762,1.50112804824368,-1.61468035702652));
#15825=CARTESIAN_POINT('Ctrl Pts',(90.4493944441774,1.49651980955262,-1.61892455710779));
#15826=CARTESIAN_POINT('Ctrl Pts',(90.4450546253874,1.44095692598081,-1.67009812054065));
#15827=CARTESIAN_POINT('Ctrl Pts',(90.4406352299576,1.38264828060835,-1.71845427083435));
#15828=CARTESIAN_POINT('Ctrl Pts',(90.4362128090986,1.3219392900851,-1.76372396404811));
#15829=CARTESIAN_POINT('Ctrl Pts',(90.4318748345868,1.2623895407686,-1.80812923020853));
#15830=CARTESIAN_POINT('Ctrl Pts',(90.4275342347738,1.20053049057327,-1.8495651987225));
#15831=CARTESIAN_POINT('Ctrl Pts',(90.4232444676202,1.13670532799525,-1.88781504244614));
#15832=CARTESIAN_POINT('Ctrl Pts',(90.4189572002254,1.0729173579975,-1.92604259699218));
#15833=CARTESIAN_POINT('Ctrl Pts',(90.4147208685469,1.00716565231536,-1.96108787795614));
#15834=CARTESIAN_POINT('Ctrl Pts',(90.4105665447433,0.939807813952254,-1.99276793951803));
#15835=CARTESIAN_POINT('Ctrl Pts',(90.406413233415,0.872466391775119,-2.02444028014061));
#15836=CARTESIAN_POINT('Ctrl Pts',(90.4023419306153,0.80351966725319,-2.05274904906297));
#15837=CARTESIAN_POINT('Ctrl Pts',(90.3983599093118,0.733339033107106,-2.07754385959433));
#15838=CARTESIAN_POINT('Ctrl Pts',(90.3942374240011,0.660682808715153,-2.10321329589457));
#15839=CARTESIAN_POINT('Ctrl Pts',(90.3902107121892,0.586704040681358,-2.12511616524922));
#15840=CARTESIAN_POINT('Ctrl Pts',(90.386261178544,0.511830009240368,-2.14312305697451));
#15841=CARTESIAN_POINT('Ctrl Pts',(90.3824419404883,0.439426081094696,-2.16053589917779));
#15842=CARTESIAN_POINT('Ctrl Pts',(90.3786945635058,0.366185095016135,-2.17430556237347));
#15843=CARTESIAN_POINT('Ctrl Pts',(90.3749798984358,0.292506650500107,-2.18435136400926));
#15844=CARTESIAN_POINT('Ctrl Pts',(90.3710751413363,0.215057829709192,-2.19491124343806));
#15845=CARTESIAN_POINT('Ctrl Pts',(90.367206325069,0.137125588283632,-2.20135558254538));
#15846=CARTESIAN_POINT('Ctrl Pts',(90.3633062801793,0.0591887388210525,
-2.20363835003113));
#15847=CARTESIAN_POINT('Ctrl Pts',(90.359781207124,-0.0112548319128014,
-2.20570163965549));
#15848=CARTESIAN_POINT('Ctrl Pts',(90.3562300839869,-0.0817028455918926,
-2.20436504621134));
#15849=CARTESIAN_POINT('Ctrl Pts',(90.3525926877338,-0.151789755927138,
-2.19963533387595));
#15850=CARTESIAN_POINT('Ctrl Pts',(90.3522060658021,-0.159239353050694,
-2.19913260874168));
#15851=CARTESIAN_POINT('Ctrl Pts',(90.3518184691787,-0.166684913452266,
-2.19859157174713));
#15852=CARTESIAN_POINT('Ctrl Pts',(90.3514298255451,-0.174126029259769,
-2.19801224645037));
#15853=CARTESIAN_POINT('',(90.3498698986825,-0.214101726762253,-2.19357617843498));
#15854=CARTESIAN_POINT('Ctrl Pts',(90.3519463663221,-0.174082286703647,
-2.19711432507641));
#15855=CARTESIAN_POINT('Ctrl Pts',(90.3516028176952,-0.180756616910668,
-2.19658550295199));
#15856=CARTESIAN_POINT('Ctrl Pts',(90.3512580795196,-0.187428441846501,
-2.1960262757715));
#15857=CARTESIAN_POINT('Ctrl Pts',(90.3505659730386,-0.200768470428712,
-2.19484688993294));
#15858=CARTESIAN_POINT('Ctrl Pts',(90.3502186079292,-0.207436597587503,
-2.1942267214521));
#15859=CARTESIAN_POINT('Ctrl Pts',(90.3498698986825,-0.214101726762254,
-2.19357617843498));
#15860=CARTESIAN_POINT('',(90.3498698986825,-2.69912154532077E-16,2.204));
#15861=CARTESIAN_POINT('Origin',(90.3498698986825,0.,0.));
#15862=CARTESIAN_POINT('',(33.4926516271063,2.69912154532077E-16,2.204));
#15863=CARTESIAN_POINT('',(66.9212607628943,-2.69912154532077E-16,2.204));
#15864=CARTESIAN_POINT('Origin',(33.4926516271063,0.,0.));
#15865=CARTESIAN_POINT('',(90.3498698986825,1.62325119196235,-1.49086269246796));
#15866=CARTESIAN_POINT('Origin',(90.3498698986825,0.,0.));
#15867=CARTESIAN_POINT('Ctrl Pts',(90.3498698986825,1.62325119196235,-1.49086269246796));
#15868=CARTESIAN_POINT('Ctrl Pts',(90.3540342343737,1.67526300385128,-1.43423223543702));
#15869=CARTESIAN_POINT('Ctrl Pts',(90.358198570065,1.72434765652125,-1.37483397863705));
#15870=CARTESIAN_POINT('Ctrl Pts',(90.3623629057562,1.77021263623129,-1.31299779989422));
#15871=CARTESIAN_POINT('Ctrl Pts',(90.366524563556,1.8160481222971,-1.25120138513401));
#15872=CARTESIAN_POINT('Ctrl Pts',(90.3706862213558,1.8586677886908,-1.18697052503797));
#15873=CARTESIAN_POINT('Ctrl Pts',(90.3748478791556,1.89781988675447,-1.120667514225));
#15874=CARTESIAN_POINT('Ctrl Pts',(90.379009024366,1.93696716247229,-1.05437266992329));
#15875=CARTESIAN_POINT('Ctrl Pts',(90.3831701695763,1.97264748370526,-0.98600656164491));
#15876=CARTESIAN_POINT('Ctrl Pts',(90.3873313147867,2.00465335684887,-0.915959015936052));
#15877=CARTESIAN_POINT('Ctrl Pts',(90.3914923669492,2.03665851430572,-0.845913036567883));
#15878=CARTESIAN_POINT('Ctrl Pts',(90.3956534191117,2.06498920101561,-0.774186100698475));
#15879=CARTESIAN_POINT('Ctrl Pts',(90.3998144712743,2.08948530986951,-0.701189803005941));
#15880=CARTESIAN_POINT('Ctrl Pts',(90.4039765044813,2.11398719413109,-0.628176295095227));
#15881=CARTESIAN_POINT('Ctrl Pts',(90.4081385376883,2.13465256077998,-0.553893253843861));
#15882=CARTESIAN_POINT('Ctrl Pts',(90.4123005708953,2.15137097947947,-0.478768115744507));
#15883=CARTESIAN_POINT('Ctrl Pts',(90.4164646600594,2.16809765672722,-0.403605867402304));
#15884=CARTESIAN_POINT('Ctrl Pts',(90.4206287492236,2.18087341220672,-0.327601130908672));
#15885=CARTESIAN_POINT('Ctrl Pts',(90.4247928383877,2.1896390276492,-0.251191020133017));
#15886=CARTESIAN_POINT('Ctrl Pts',(90.4289632381674,2.19841792725226,-0.174665110964433));
#15887=CARTESIAN_POINT('Ctrl Pts',(90.4331336379471,2.203174502206,-0.0977330455384561));
#15888=CARTESIAN_POINT('Ctrl Pts',(90.4373040377268,2.20390150594005,-0.0208363172176138));
#15889=CARTESIAN_POINT('Ctrl Pts',(90.4414778779445,2.20462910942745,0.056123848288982));
#15890=CARTESIAN_POINT('Ctrl Pts',(90.4456517181622,2.20132053768274,0.133048172453329));
#15891=CARTESIAN_POINT('Ctrl Pts',(90.4498255583799,2.19402060648631,0.20949839692337));
#15892=CARTESIAN_POINT('Ctrl Pts',(90.4540074390487,2.18670661276303,0.286095894471075));
#15893=CARTESIAN_POINT('Ctrl Pts',(90.4581893197175,2.17538596621945,0.362217025950471));
#15894=CARTESIAN_POINT('Ctrl Pts',(90.4623712003864,2.16015491417952,0.437431990995269));
#15895=CARTESIAN_POINT('Ctrl Pts',(90.4645876718248,2.15208218458796,0.477297265728303));
#15896=CARTESIAN_POINT('Ctrl Pts',(90.4668041432632,2.14291180085852,0.516908206597404));
#15897=CARTESIAN_POINT('Ctrl Pts',(90.4690206147016,2.13266372326016,0.55620270000255));
#15898=CARTESIAN_POINT('Ctrl Pts',(90.473057969927,2.11399660717457,0.627778550485544));
#15899=CARTESIAN_POINT('Ctrl Pts',(90.4770953251523,2.09167923412068,0.698577635480653));
#15900=CARTESIAN_POINT('Ctrl Pts',(90.4811326803776,2.06579110704165,0.768194703228045));
#15901=CARTESIAN_POINT('Ctrl Pts',(90.4851634929537,2.03994493241042,0.837698954532925));
#15902=CARTESIAN_POINT('Ctrl Pts',(90.4891943055299,2.01053965260703,0.906024537409715));
#15903=CARTESIAN_POINT('Ctrl Pts',(90.493225118106,1.97770533275813,0.972778297856222));
#15904=CARTESIAN_POINT('Ctrl Pts',(90.4972504974604,1.94491527101734,1.03944207942818));
#15905=CARTESIAN_POINT('Ctrl Pts',(90.5012758768148,1.90870556178229,1.10453781181376));
#15906=CARTESIAN_POINT('Ctrl Pts',(90.5053012561693,1.86925480157049,1.16769109220105));
#15907=CARTESIAN_POINT('Ctrl Pts',(90.5093236563983,1.82983323829924,1.23079763375331));
#15908=CARTESIAN_POINT('Ctrl Pts',(90.5133460566273,1.78717563777286,1.291964162283));
#15909=CARTESIAN_POINT('Ctrl Pts',(90.5173684568564,1.74150642743007,1.35084098369118));
#15910=CARTESIAN_POINT('Ctrl Pts',(90.5213892394597,1.6958555831581,1.40969412753051));
#15911=CARTESIAN_POINT('Ctrl Pts',(90.5254100220631,1.64719583023854,1.46625900656898));
#15912=CARTESIAN_POINT('Ctrl Pts',(90.5294308046664,1.59579380100114,1.52021647954702));
#15913=CARTESIAN_POINT('Ctrl Pts',(90.5334513289884,1.54439507365432,1.57417048648151));
#15914=CARTESIAN_POINT('Ctrl Pts',(90.5374718533105,1.49025475691073,1.62551706820624));
#15915=CARTESIAN_POINT('Ctrl Pts',(90.5414923776325,1.43367730249767,1.67397293655035));
#15916=CARTESIAN_POINT('Ctrl Pts',(90.545516831533,1.37704455043435,1.72247616467211));
#15917=CARTESIAN_POINT('Ctrl Pts',(90.5495412854335,1.31797027415438,1.76808271884422));
#15918=CARTESIAN_POINT('Ctrl Pts',(90.553565739334,1.25679240448188,1.81054932328193));
#15919=CARTESIAN_POINT('Ctrl Pts',(90.5575921261865,1.19558515097667,1.85303632450049));
#15920=CARTESIAN_POINT('Ctrl Pts',(90.5616185130389,1.1322727072202,1.8923801166326));
#15921=CARTESIAN_POINT('Ctrl Pts',(90.5656448998913,1.06722004242361,1.92838206303869));
#15922=CARTESIAN_POINT('Ctrl Pts',(90.5696786738581,1.0020480270792,1.96445006134349));
#15923=CARTESIAN_POINT('Ctrl Pts',(90.5737124478249,0.935129852251466,1.99716375370825));
#15924=CARTESIAN_POINT('Ctrl Pts',(90.5777462217918,0.866852550327255,2.02637179609052));
#15925=CARTESIAN_POINT('Ctrl Pts',(90.5812212581014,0.808032669673591,2.0515340904202));
#15926=CARTESIAN_POINT('Ctrl Pts',(90.5846962944111,0.748204602075248,2.07409538561612));
#15927=CARTESIAN_POINT('Ctrl Pts',(90.5881713307208,0.687623727431014,2.09398892295873));
#15928=CARTESIAN_POINT('Ctrl Pts',(90.5930975172393,0.60174471456295,2.12218985864133));
#15929=CARTESIAN_POINT('Ctrl Pts',(90.5980237037578,0.514066413824007,2.14512431597063));
#15930=CARTESIAN_POINT('Ctrl Pts',(90.6029498902764,0.425177719435792,2.16260026516584));
#15931=CARTESIAN_POINT('Ctrl Pts',(90.6078130617383,0.337426076211533,2.1798526645777));
#15932=CARTESIAN_POINT('Ctrl Pts',(90.6126762332001,0.248494831068513,2.19178526875751));
#15933=CARTESIAN_POINT('Ctrl Pts',(90.617539404662,0.158971471143045,2.19825932759595));
#15934=CARTESIAN_POINT('Ctrl Pts',(90.6203755450525,0.106762574342893,2.20203491723039));
#15935=CARTESIAN_POINT('Ctrl Pts',(90.6232116854429,0.0543526856127783,
2.20395487670908));
#15936=CARTESIAN_POINT('Ctrl Pts',(90.6260478258334,0.0018616288768175,
2.20399921377888));
#15937=CARTESIAN_POINT('',(70.8,1.96408146470558,0.999999999999996));
#15938=CARTESIAN_POINT('',(69.8,2.204,1.22464679914735E-16));
#15939=CARTESIAN_POINT('Ctrl Pts',(70.8,1.96408146470558,0.999999999999995));
#15940=CARTESIAN_POINT('Ctrl Pts',(70.6722659399236,1.96408146470558,0.999999999999995));
#15941=CARTESIAN_POINT('Ctrl Pts',(70.5375729856138,1.97786636144381,0.974089083852149));
#15942=CARTESIAN_POINT('Ctrl Pts',(70.2919072356979,2.02515309008955,0.871527146747205));
#15943=CARTESIAN_POINT('Ctrl Pts',(70.1807303328797,2.05773682352636,0.794943895252836));
#15944=CARTESIAN_POINT('Ctrl Pts',(70.0052106451649,2.11719154668924,0.619424207537946));
#15945=CARTESIAN_POINT('Ctrl Pts',(69.9285120447932,2.14824329851503,0.508191937532767));
#15946=CARTESIAN_POINT('Ctrl Pts',(69.8258593644549,2.19189597286799,0.262298234370078));
#15947=CARTESIAN_POINT('Ctrl Pts',(69.8,2.204,0.127509325063069));
#15948=CARTESIAN_POINT('Ctrl Pts',(69.8,2.204,-1.04083408558608E-15));
#15949=CARTESIAN_POINT('Ctrl Pts',(69.8,2.204,9.36750677027476E-16));
#15950=CARTESIAN_POINT('Ctrl Pts',(69.8,2.204,-0.12750932506307));
#15951=CARTESIAN_POINT('Ctrl Pts',(69.8258593644549,2.19189597286799,-0.262298234370079));
#15952=CARTESIAN_POINT('Ctrl Pts',(69.9285120447932,2.14824329851503,-0.508191937532767));
#15953=CARTESIAN_POINT('Ctrl Pts',(70.0052106451649,2.11719154668924,-0.619424207537946));
#15954=CARTESIAN_POINT('Ctrl Pts',(70.1807303328797,2.05773682352636,-0.794943895252837));
#15955=CARTESIAN_POINT('Ctrl Pts',(70.2919072356979,2.02515309008955,-0.871527146747215));
#15956=CARTESIAN_POINT('Ctrl Pts',(70.5375729856138,1.97786636144381,-0.974089083852154));
#15957=CARTESIAN_POINT('Ctrl Pts',(70.6722659399236,1.96408146470558,-0.999999999999996));
#15958=CARTESIAN_POINT('Ctrl Pts',(70.9277340600764,1.96408146470558,-0.999999999999996));
#15959=CARTESIAN_POINT('Ctrl Pts',(71.0624270143862,1.97786636144381,-0.974089083852144));
#15960=CARTESIAN_POINT('Ctrl Pts',(71.3080927643021,2.02515309008955,-0.871527146747202));
#15961=CARTESIAN_POINT('Ctrl Pts',(71.4192696671203,2.05773682352636,-0.794943895252837));
#15962=CARTESIAN_POINT('Ctrl Pts',(71.5947893548351,2.11719154668924,-0.619424207537946));
#15963=CARTESIAN_POINT('Ctrl Pts',(71.6714879552068,2.14824329851503,-0.508191937532762));
#15964=CARTESIAN_POINT('Ctrl Pts',(71.7741406355451,2.19189597286799,-0.262298234370079));
#15965=CARTESIAN_POINT('Ctrl Pts',(71.8,2.204,-0.127509325063071));
#15966=CARTESIAN_POINT('Ctrl Pts',(71.8,2.204,0.12750932506307));
#15967=CARTESIAN_POINT('Ctrl Pts',(71.7741406355451,2.19189597286799,0.262298234370079));
#15968=CARTESIAN_POINT('Ctrl Pts',(71.6714879552068,2.14824329851503,0.508191937532767));
#15969=CARTESIAN_POINT('Ctrl Pts',(71.5947893548351,2.11719154668924,0.619424207537946));
#15970=CARTESIAN_POINT('Ctrl Pts',(71.4192696671203,2.05773682352636,0.794943895252837));
#15971=CARTESIAN_POINT('Ctrl Pts',(71.3080927643021,2.02515309008955,0.871527146747205));
#15972=CARTESIAN_POINT('Ctrl Pts',(71.0624270143862,1.97786636144381,0.974089083852149));
#15973=CARTESIAN_POINT('Ctrl Pts',(70.9277340600764,1.96408146470558,0.999999999999996));
#15974=CARTESIAN_POINT('Ctrl Pts',(70.8,1.96408146470558,0.999999999999996));
#15975=CARTESIAN_POINT('Origin',(66.9212607628943,0.,0.));
#15976=CARTESIAN_POINT('',(91.4824158962551,-3.3646198792706E-12,2.204));
#15977=CARTESIAN_POINT('',(91.3776298668357,4.55134372080087E-12,2.204));
#15978=CARTESIAN_POINT('',(66.9212607628943,-2.69912154532077E-16,2.204));
#15979=CARTESIAN_POINT('Ctrl Pts',(91.4824158962551,-3.3646198792706E-12,
2.204));
#15980=CARTESIAN_POINT('Ctrl Pts',(91.4801781402797,0.0394543598407125,
2.20400000000006));
#15981=CARTESIAN_POINT('Ctrl Pts',(91.4779713869581,0.0789033116011558,
2.20294058194433));
#15982=CARTESIAN_POINT('Ctrl Pts',(91.4749196852296,0.134210744976245,2.1999675487167));
#15983=CARTESIAN_POINT('Ctrl Pts',(91.4740474214224,0.150107529048946,2.19894008286232));
#15984=CARTESIAN_POINT('Ctrl Pts',(91.4725385729675,0.177755683031999,2.19685185866944));
#15985=CARTESIAN_POINT('Ctrl Pts',(91.4718995767405,0.189512119582209,2.19586892502936));
#15986=CARTESIAN_POINT('Ctrl Pts',(91.4705665597984,0.214133982223726,2.19361112414296));
#15987=CARTESIAN_POINT('Ctrl Pts',(91.4698731598011,0.226997251520984,2.19231735475216));
#15988=CARTESIAN_POINT('Ctrl Pts',(91.4682214240739,0.257766309931557,2.18894893085676));
#15989=CARTESIAN_POINT('Ctrl Pts',(91.4672664776349,0.275659637616388,2.18676763340557));
#15990=CARTESIAN_POINT('Ctrl Pts',(91.4639474872967,0.338186307846201,2.17836560523575));
#15991=CARTESIAN_POINT('Ctrl Pts',(91.4616194683117,0.382655249285325,2.17099562685355));
#15992=CARTESIAN_POINT('Ctrl Pts',(91.4559115143877,0.492756803489202,2.14925966686931));
#15993=CARTESIAN_POINT('Ctrl Pts',(91.4525792516709,0.558018222403516,2.13324702402587));
#15994=CARTESIAN_POINT('Ctrl Pts',(91.4423562410431,0.758380775879455,2.0742597226521));
#15995=CARTESIAN_POINT('Ctrl Pts',(91.4356619409826,0.890127883662804,2.02122821920269));
#15996=CARTESIAN_POINT('Ctrl Pts',(91.4256608296784,1.06843326519412,1.92861997232397));
#15997=CARTESIAN_POINT('Ctrl Pts',(91.4226505681136,1.11987386384554,1.89921196367638));
#15998=CARTESIAN_POINT('Ctrl Pts',(91.418782576099,1.18197488347845,1.86030882788842));
#15999=CARTESIAN_POINT('Ctrl Pts',(91.418034226323,1.19381429645149,1.85273337679333));
#16000=CARTESIAN_POINT('Ctrl Pts',(91.4168465492248,1.21230993013197,1.84064805438785));
#16001=CARTESIAN_POINT('Ctrl Pts',(91.4164120628725,1.21901550713279,1.83621398970867));
#16002=CARTESIAN_POINT('Ctrl Pts',(91.4155854183853,1.23165467731864,1.82775658928307));
#16003=CARTESIAN_POINT('Ctrl Pts',(91.4151937531492,1.23759307706115,1.8237408708577));
#16004=CARTESIAN_POINT('Ctrl Pts',(91.4142594981588,1.25164198962775,1.81414037494941));
#16005=CARTESIAN_POINT('Ctrl Pts',(91.4137152302728,1.25973480475251,1.80853011707421));
#16006=CARTESIAN_POINT('Ctrl Pts',(91.4118607479087,1.28701252139134,1.78934821077243));
#16007=CARTESIAN_POINT('Ctrl Pts',(91.4105349742071,1.30601725021243,1.77552445805128));
#16008=CARTESIAN_POINT('Ctrl Pts',(91.4072327079099,1.3522561000108,1.74074697169256));
#16009=CARTESIAN_POINT('Ctrl Pts',(91.4052391501105,1.37922776628106,1.71945547580777));
#16010=CARTESIAN_POINT('Ctrl Pts',(91.3964224042232,1.49497838962054,1.62360553138485));
#16011=CARTESIAN_POINT('Ctrl Pts',(91.3893940912104,1.57829249398324,1.54274017667738));
#16012=CARTESIAN_POINT('Ctrl Pts',(91.3750887937157,1.73622748421512,1.3631975731532));
#16013=CARTESIAN_POINT('Ctrl Pts',(91.3678528592593,1.80970648731728,1.26402655137352));
#16014=CARTESIAN_POINT('Ctrl Pts',(91.3591979627015,1.89075204382571,1.13297187962658));
#16015=CARTESIAN_POINT('Ctrl Pts',(91.3574839966505,1.90643258991293,1.10638306549075));
#16016=CARTESIAN_POINT('Ctrl Pts',(91.3549239995837,1.92928036877724,1.06571214141963));
#16017=CARTESIAN_POINT('Ctrl Pts',(91.3540631744631,1.93686275312465,1.05186871973477));
#16018=CARTESIAN_POINT('Ctrl Pts',(91.3525243078238,1.95023304031517,1.02682326907866));
#16019=CARTESIAN_POINT('Ctrl Pts',(91.3518443765184,1.95607471014771,1.01565086274235));
#16020=CARTESIAN_POINT('Ctrl Pts',(91.3503974079138,1.96836276081221,0.991650209408952));
#16021=CARTESIAN_POINT('Ctrl Pts',(91.3496314056636,1.97478033298395,0.978807818604067));
#16022=CARTESIAN_POINT('Ctrl Pts',(91.34754902315,1.99198104901975,0.943529076235189));
#16023=CARTESIAN_POINT('Ctrl Pts',(91.3462414464137,2.00251046811188,0.920970959756128));
#16024=CARTESIAN_POINT('Ctrl Pts',(91.336926036561,2.07547225740982,0.757487723957267));
#16025=CARTESIAN_POINT('Ctrl Pts',(91.329443973503,2.12335272623722,0.610534215965251));
#16026=CARTESIAN_POINT('Ctrl Pts',(91.3154590438008,2.18371514442958,0.327543255072804));
#16027=CARTESIAN_POINT('Ctrl Pts',(91.3089636843362,2.19968962679294,0.193012387603668));
#16028=CARTESIAN_POINT('Ctrl Pts',(91.3009677739356,2.2037152438386,0.0397857276844529));
#16029=CARTESIAN_POINT('Ctrl Pts',(91.300013456607,2.20396769519286,0.0216826630416138));
#16030=CARTESIAN_POINT('Ctrl Pts',(91.2985665448823,2.20401174040237,-0.00544011018295865));
#16031=CARTESIAN_POINT('Ctrl Pts',(91.2980825714011,2.2039710236282,-0.0144591830885269));
#16032=CARTESIAN_POINT('Ctrl Pts',(91.2972039685478,2.20379769732076,-0.0307295685720725));
#16033=CARTESIAN_POINT('Ctrl Pts',(91.2968104085057,2.20368464963887,-0.0379810569206739));
#16034=CARTESIAN_POINT('Ctrl Pts',(91.295996679291,2.20337850948319,-0.0528951323439904));
#16035=CARTESIAN_POINT('Ctrl Pts',(91.2955762981024,2.20318123234762,-0.0605574505010265));
#16036=CARTESIAN_POINT('Ctrl Pts',(91.2944730727269,2.20256178718748,-0.0805608770538496));
#16037=CARTESIAN_POINT('Ctrl Pts',(91.2937868365485,2.2020758697894,-0.0928995722403264));
#16038=CARTESIAN_POINT('Ctrl Pts',(91.2906575360942,2.19940691485961,-0.148734287476722));
#16039=CARTESIAN_POINT('Ctrl Pts',(91.2881578825651,2.1960387436545,-0.192161395489317));
#16040=CARTESIAN_POINT('Ctrl Pts',(91.2805869618852,2.18216995964079,-0.32123739224586));
#16041=CARTESIAN_POINT('Ctrl Pts',(91.275407878687,2.16792481370537,-0.406398663174594));
#16042=CARTESIAN_POINT('Ctrl Pts',(91.2604311365895,2.11244703903914,-0.649428606466381));
#16043=CARTESIAN_POINT('Ctrl Pts',(91.250710854518,2.05864191430014,-0.803865237988029));
#16044=CARTESIAN_POINT('Ctrl Pts',(91.2400206920276,1.97644576677972,-0.975720710666994));
#16045=CARTESIAN_POINT('Ctrl Pts',(91.2384965382159,1.96414602370372,-1.00024960259684));
#16046=CARTESIAN_POINT('Ctrl Pts',(91.2360889387296,1.94378590658349,-1.03902839588803));
#16047=CARTESIAN_POINT('Ctrl Pts',(91.2351953297012,1.93601954951955,-1.05342867928696));
#16048=CARTESIAN_POINT('Ctrl Pts',(91.2336179184206,1.92193856320357,-1.07885567519416));
#16049=CARTESIAN_POINT('Ctrl Pts',(91.23293188587,1.91568763550544,-1.08991664875825));
#16050=CARTESIAN_POINT('Ctrl Pts',(91.2315037355365,1.90240995760003,-1.11294425046954));
#16051=CARTESIAN_POINT('Ctrl Pts',(91.230762311013,1.89536511547899,-1.12489983666365));
#16052=CARTESIAN_POINT('Ctrl Pts',(91.2288213843301,1.87652588338641,-1.15619184060402));
#16053=CARTESIAN_POINT('Ctrl Pts',(91.2276287173098,1.86454537908809,-1.17541462598263));
#16054=CARTESIAN_POINT('Ctrl Pts',(91.2217305794806,1.80331407730494,-1.27036790582983));
#16055=CARTESIAN_POINT('Ctrl Pts',(91.2171888958627,1.74973425701063,-1.34320833345299));
#16056=CARTESIAN_POINT('Ctrl Pts',(91.2081357489223,1.63181796360114,-1.48443722380726));
#16057=CARTESIAN_POINT('Ctrl Pts',(91.2036405300379,1.56728530893299,-1.55241775699004));
#16058=CARTESIAN_POINT('Ctrl Pts',(91.1977522743822,1.47814337143887,-1.63508054515882));
#16059=CARTESIAN_POINT('Ctrl Pts',(91.1963959538015,1.45730292382031,-1.65368206473617));
#16060=CARTESIAN_POINT('Ctrl Pts',(91.1906734065766,1.36845661683924,-1.72999933951523));
#16061=CARTESIAN_POINT('Ctrl Pts',(91.1862372482116,1.29733928572496,-1.78395035269217));
#16062=CARTESIAN_POINT('Ctrl Pts',(91.180749987825,1.21063959493721,-1.84179103655169));
#16063=CARTESIAN_POINT('Ctrl Pts',(91.179950438576,1.19803652024295,-1.8500137628203));
#16064=CARTESIAN_POINT('Ctrl Pts',(91.1786948322767,1.17831612219093,-1.86259408827682));
#16065=CARTESIAN_POINT('Ctrl Pts',(91.1782444438249,1.1712563536404,-1.8670415557535));
#16066=CARTESIAN_POINT('Ctrl Pts',(91.1774054345939,1.15813586424978,-1.87520341503529));
#16067=CARTESIAN_POINT('Ctrl Pts',(91.1770175288974,1.15208223324073,-1.87892869771563));
#16068=CARTESIAN_POINT('Ctrl Pts',(91.176116045132,1.13804140460854,-1.88747577598316));
#16069=CARTESIAN_POINT('Ctrl Pts',(91.1756011282147,1.13004152511208,-1.89227619246865));
#16070=CARTESIAN_POINT('Ctrl Pts',(91.173945446253,1.10437265942562,-1.907458256576));
#16071=CARTESIAN_POINT('Ctrl Pts',(91.1727931761148,1.08658974413816,-1.91764403316666));
#16072=CARTESIAN_POINT('Ctrl Pts',(91.1663870173423,0.987996445036268,-1.97230506420663));
#16073=CARTESIAN_POINT('Ctrl Pts',(91.1609074946563,0.904602956887268,-2.01191822435199));
#16074=CARTESIAN_POINT('Ctrl Pts',(91.145420579204,0.664707189880399,-2.10793589015116));
#16075=CARTESIAN_POINT('Ctrl Pts',(91.135397274314,0.503920223382356,-2.15204740998207));
#16076=CARTESIAN_POINT('Ctrl Pts',(91.1234505367509,0.296591852644385,-2.18438823761559));
#16077=CARTESIAN_POINT('Ctrl Pts',(91.1210043986397,0.253301082733593,-2.18983050493573));
#16078=CARTESIAN_POINT('Ctrl Pts',(91.1175898111436,0.191676504015374,-2.19572546887252));
#16079=CARTESIAN_POINT('Ctrl Pts',(91.116588542128,0.17345665490953,-2.19723986723269));
#16080=CARTESIAN_POINT('Ctrl Pts',(91.1148957197791,0.142403616795862,-2.19943226310102));
#16081=CARTESIAN_POINT('Ctrl Pts',(91.1142006037765,0.129579708798338,-2.20022502915049));
#16082=CARTESIAN_POINT('Ctrl Pts',(91.1127941258068,0.10348776321749,-2.2016091044885));
#16083=CARTESIAN_POINT('Ctrl Pts',(91.1120830330832,0.0902198379230107,
-2.202192715812));
#16084=CARTESIAN_POINT('Ctrl Pts',(91.1103197421546,0.0571356243412686,
-2.20334847441452));
#16085=CARTESIAN_POINT('Ctrl Pts',(91.1092721809343,0.0373151597815744,
-2.20377326244858));
#16086=CARTESIAN_POINT('Ctrl Pts',(91.1051597604413,-0.0411051475227443,
-2.20439563534501));
#16087=CARTESIAN_POINT('Ctrl Pts',(91.1021591586453,-0.0996994388175074,
-2.20252367159185));
#16088=CARTESIAN_POINT('Ctrl Pts',(91.0941803563011,-0.258039267611667,
-2.19113227467141));
#16089=CARTESIAN_POINT('Ctrl Pts',(91.0893220315997,-0.357323449568237,
-2.17714639031626));
#16090=CARTESIAN_POINT('Ctrl Pts',(91.077652638277,-0.593504242587038,-2.12727907218789));
#16091=CARTESIAN_POINT('Ctrl Pts',(91.07089026408,-0.728553107449761,-2.08488961658958));
#16092=CARTESIAN_POINT('Ctrl Pts',(91.0624947438596,-0.876660070092227,
-2.02224320879027));
#16093=CARTESIAN_POINT('Ctrl Pts',(91.0614594181588,-0.894615674425303,
-2.01436422145357));
#16094=CARTESIAN_POINT('Ctrl Pts',(91.0599201315754,-0.920805593069546,
-2.0024527590993));
#16095=CARTESIAN_POINT('Ctrl Pts',(91.0594268475946,-0.929124142751027,
-1.99860659309374));
#16096=CARTESIAN_POINT('Ctrl Pts',(91.0585462936461,-0.943835430528812,
-1.99169298692826));
#16097=CARTESIAN_POINT('Ctrl Pts',(91.0581602939695,-0.950237685206415,
-1.98864642759259));
#16098=CARTESIAN_POINT('Ctrl Pts',(91.0573099592901,-0.964238339005941,
-1.98190106652062));
#16099=CARTESIAN_POINT('Ctrl Pts',(91.0568448713887,-0.97183010081582,-1.97818949096239));
#16100=CARTESIAN_POINT('Ctrl Pts',(91.0554912421186,-0.993743049685785,
-1.96731977234564));
#16101=CARTESIAN_POINT('Ctrl Pts',(91.0545961614286,-1.00800752955069,-1.96004926605665));
#16102=CARTESIAN_POINT('Ctrl Pts',(91.0525252856672,-1.0405336461502,-1.94302197192162));
#16103=CARTESIAN_POINT('Ctrl Pts',(91.0513442365129,-1.05873938360277,-1.93316205039062));
#16104=CARTESIAN_POINT('Ctrl Pts',(91.047314576823,-1.11980957672644,-1.89896603481867));
#16105=CARTESIAN_POINT('Ctrl Pts',(91.0444165918693,-1.16199416767576,-1.87344990124736));
#16106=CARTESIAN_POINT('Ctrl Pts',(91.0358744265014,-1.28243541750431,-1.79496527203492));
#16107=CARTESIAN_POINT('Ctrl Pts',(91.0301610603921,-1.35818659783151,-1.73835268346984));
#16108=CARTESIAN_POINT('Ctrl Pts',(91.0166397242476,-1.53026215195349,-1.59161903700953));
#16109=CARTESIAN_POINT('Ctrl Pts',(91.0089325982786,-1.62260729679554,-1.49736706598294));
#16110=CARTESIAN_POINT('Ctrl Pts',(91.0002374767894,-1.72142699463182,-1.37655338591616));
#16111=CARTESIAN_POINT('Ctrl Pts',(90.9988920432473,-1.73654568698149,-1.357431127749));
#16112=CARTESIAN_POINT('Ctrl Pts',(90.9967730952672,-1.76007287796891,-1.32663716327648));
#16113=CARTESIAN_POINT('Ctrl Pts',(90.9959914118325,-1.76868940103444,-1.31512756613624));
#16114=CARTESIAN_POINT('Ctrl Pts',(90.9945396947139,-1.78457104247931,-1.29347509431724));
#16115=CARTESIAN_POINT('Ctrl Pts',(90.9938686005316,-1.79186381548404,-1.28335330323643));
#16116=CARTESIAN_POINT('Ctrl Pts',(90.9923620777023,-1.80812133866769,-1.26038038655201));
#16117=CARTESIAN_POINT('Ctrl Pts',(90.9915285951134,-1.81703582701421,-1.24749441469915));
#16118=CARTESIAN_POINT('Ctrl Pts',(90.9890429038808,-1.84337072472549,-1.20854583191193));
#16119=CARTESIAN_POINT('Ctrl Pts',(90.9874063314547,-1.86037365650784,-1.18220499231589));
#16120=CARTESIAN_POINT('Ctrl Pts',(90.983671473719,-1.89831876705991,-1.12057352732373));
#16121=CARTESIAN_POINT('Ctrl Pts',(90.9815874536804,-1.91884909186674,-1.08504266262503));
#16122=CARTESIAN_POINT('Ctrl Pts',(90.9741115088847,-1.9897974032026,-0.953936813325641));
#16123=CARTESIAN_POINT('Ctrl Pts',(90.9688947326589,-2.03416360030641,-0.85525970787352));
#16124=CARTESIAN_POINT('Ctrl Pts',(90.9574430381797,-2.11519846482341,-0.632588915433794));
#16125=CARTESIAN_POINT('Ctrl Pts',(90.9512277224984,-2.14856530016115,-0.507831853855941));
#16126=CARTESIAN_POINT('Ctrl Pts',(90.9434490079919,-2.17434623604072,-0.360896830609277));
#16127=CARTESIAN_POINT('Ctrl Pts',(90.9423781358766,-2.17757786439909,-0.340855780621291));
#16128=CARTESIAN_POINT('Ctrl Pts',(90.9408012221957,-2.18186962429036,-0.311681564952728));
#16129=CARTESIAN_POINT('Ctrl Pts',(90.9403068029366,-2.18315024161461,-0.302581347376627));
#16130=CARTESIAN_POINT('Ctrl Pts',(90.9394244442498,-2.18532003665806,-0.286431191430478));
#16131=CARTESIAN_POINT('Ctrl Pts',(90.9390377841379,-2.18623208691783,-0.279384592817169));
#16132=CARTESIAN_POINT('Ctrl Pts',(90.9381938896706,-2.18813860883047,-0.264073317979917));
#16133=CARTESIAN_POINT('Ctrl Pts',(90.9377359914222,-2.18912032717815,-0.255807500258446));
#16134=CARTESIAN_POINT('Ctrl Pts',(90.936424766465,-2.19178298283505,-0.23224990874765));
#16135=CARTESIAN_POINT('Ctrl Pts',(90.935565504482,-2.19335063733117,-0.216946118943796));
#16136=CARTESIAN_POINT('Ctrl Pts',(90.9282071839857,-2.20529881230776,-0.0868877893682897));
#16137=CARTESIAN_POINT('Ctrl Pts',(90.9213189656286,-2.20682480008865,0.0284918618030112));
#16138=CARTESIAN_POINT('Ctrl Pts',(90.9039493902481,-2.18800114639563,0.317090697263738));
#16139=CARTESIAN_POINT('Ctrl Pts',(90.8935353510432,-2.15614915948067,0.48881034344095));
#16140=CARTESIAN_POINT('Ctrl Pts',(90.8822945800032,-2.09654469719752,0.680307456604186));
#16141=CARTESIAN_POINT('Ctrl Pts',(90.8808241811362,-2.08821535415084,0.705460575616805));
#16142=CARTESIAN_POINT('Ctrl Pts',(90.8784747258084,-2.0740418983742,0.745808906767966));
#16143=CARTESIAN_POINT('Ctrl Pts',(90.8775865117799,-2.06847962883379,0.761099708810144));
#16144=CARTESIAN_POINT('Ctrl Pts',(90.8760170498827,-2.05828814459545,0.788179079006374));
#16145=CARTESIAN_POINT('Ctrl Pts',(90.8753336121017,-2.05372573383445,0.799991853889391));
#16146=CARTESIAN_POINT('Ctrl Pts',(90.8738977487521,-2.04387793751207,0.82484972110277));
#16147=CARTESIAN_POINT('Ctrl Pts',(90.8731461568559,-2.03856887516801,0.837884860599564));
#16148=CARTESIAN_POINT('Ctrl Pts',(90.8711480228918,-2.02404337323315,0.872593292053562));
#16149=CARTESIAN_POINT('Ctrl Pts',(90.869909075878,-2.01460367768383,0.894171520629218));
#16150=CARTESIAN_POINT('Ctrl Pts',(90.8631477842513,-1.96072913298534,1.01213717464));
#16151=CARTESIAN_POINT('Ctrl Pts',(90.8578572638919,-1.90972078764351,1.10537336309242));
#16152=CARTESIAN_POINT('Ctrl Pts',(90.8456971390052,-1.77478695955714,1.31458741267225));
#16153=CARTESIAN_POINT('Ctrl Pts',(90.8389496611619,-1.6859119404452,1.42678145541832));
#16154=CARTESIAN_POINT('Ctrl Pts',(90.8291431705938,-1.54989704771596,1.56788556714735));
#16155=CARTESIAN_POINT('Ctrl Pts',(90.8264267835324,-1.51160551479694,1.60483455939629));
#16156=CARTESIAN_POINT('Ctrl Pts',(90.8228950905254,-1.46185338111679,1.64948089127736));
#16157=CARTESIAN_POINT('Ctrl Pts',(90.8221674408116,-1.45160451634587,1.65850740966788));
#16158=CARTESIAN_POINT('Ctrl Pts',(90.8210050416147,-1.43525221602499,1.67264174370351));
#16159=CARTESIAN_POINT('Ctrl Pts',(90.820574782883,-1.42920370277016,1.67781289132827));
#16160=CARTESIAN_POINT('Ctrl Pts',(90.8197494982183,-1.41761411565941,1.68761321130275));
#16161=CARTESIAN_POINT('Ctrl Pts',(90.8193548882596,-1.41207812640553,1.69224805842509));
#16162=CARTESIAN_POINT('Ctrl Pts',(90.8184047061873,-1.39875896122519,1.70328828323127));
#16163=CARTESIAN_POINT('Ctrl Pts',(90.8178473172664,-1.39095446286669,1.70966759388672));
#16164=CARTESIAN_POINT('Ctrl Pts',(90.8159054535254,-1.36378288602652,1.73156814236291));
#16165=CARTESIAN_POINT('Ctrl Pts',(90.8145035517347,-1.34419823472349,1.74681509965974));
#16166=CARTESIAN_POINT('Ctrl Pts',(90.810969646717,-1.2947845923879,1.78396131659869));
#16167=CARTESIAN_POINT('Ctrl Pts',(90.8088176930298,-1.26465413705216,1.80544586634922));
#16168=CARTESIAN_POINT('Ctrl Pts',(90.8016372987192,-1.16348612427445,1.87380852034797));
#16169=CARTESIAN_POINT('Ctrl Pts',(90.7965151083704,-1.09027514932016,1.91733085295948));
#16170=CARTESIAN_POINT('Ctrl Pts',(90.7851061102643,-0.921540553026482,
2.00484417933294));
#16171=CARTESIAN_POINT('Ctrl Pts',(90.7788449753409,-0.825006131776845,
2.0464616730939));
#16172=CARTESIAN_POINT('Ctrl Pts',(90.7691859279851,-0.667240068742853,
2.10149039191718));
#16173=CARTESIAN_POINT('Ctrl Pts',(90.7656656586162,-0.607772480574641,
2.11945390409258));
#16174=CARTESIAN_POINT('Ctrl Pts',(90.7610708726807,-0.527427312167493,
2.14006333019295));
#16175=CARTESIAN_POINT('Ctrl Pts',(90.7599251863802,-0.507160438180113,
2.14495663334007));
#16176=CARTESIAN_POINT('Ctrl Pts',(90.7580523622403,-0.473652088144785,
2.15254550985492));
#16177=CARTESIAN_POINT('Ctrl Pts',(90.7573199193736,-0.460450145187544,
2.15540811629268));
#16178=CARTESIAN_POINT('Ctrl Pts',(90.7558963198507,-0.434603938493177,
2.16076409692801));
#16179=CARTESIAN_POINT('Ctrl Pts',(90.7552048430207,-0.421962498429916,
2.16326829717963));
#16180=CARTESIAN_POINT('Ctrl Pts',(90.7538373225898,-0.396792261417112,
2.16802535117414));
#16181=CARTESIAN_POINT('Ctrl Pts',(90.7531612201785,-0.384264475209838,
2.17028082153423));
#16182=CARTESIAN_POINT('Ctrl Pts',(90.7515843459321,-0.354855740132947,
2.17531286319527));
#16183=CARTESIAN_POINT('Ctrl Pts',(90.7506863348501,-0.337960493038073,
2.17800169322356));
#16184=CARTESIAN_POINT('Ctrl Pts',(90.7478362013182,-0.283891309002596,
2.18596233051483));
#16185=CARTESIAN_POINT('Ctrl Pts',(90.7459069744405,-0.246612401598594,
2.19048125144737));
#16186=CARTESIAN_POINT('Ctrl Pts',(90.7404580552706,-0.139689516270678,
2.20067793500518));
#16187=CARTESIAN_POINT('Ctrl Pts',(90.7370029463319,-0.0698659755842112,
2.20399999999936));
#16188=CARTESIAN_POINT('Ctrl Pts',(90.7335918111184,-2.00577712042713E-11,
2.204));
#16189=CARTESIAN_POINT('Ctrl Pts',(90.6267804315841,0.00190491555487048,
2.2039991767913));
#16190=CARTESIAN_POINT('Ctrl Pts',(90.6326452887204,-0.097354835602562,
2.20408496695218));
#16191=CARTESIAN_POINT('Ctrl Pts',(90.6383718140951,-0.196518494825245,
2.1974653855676));
#16192=CARTESIAN_POINT('Ctrl Pts',(90.6448581573574,-0.312104610835634,
2.18185877429554));
#16193=CARTESIAN_POINT('Ctrl Pts',(90.6458167394167,-0.329270238770531,
2.17933433254394));
#16194=CARTESIAN_POINT('Ctrl Pts',(90.6474799876175,-0.359196947643492,
2.17457153049561));
#16195=CARTESIAN_POINT('Ctrl Pts',(90.6481874099946,-0.371971262077163,
2.17242288208958));
#16196=CARTESIAN_POINT('Ctrl Pts',(90.6496052293846,-0.397662593043945,
2.16786832508738));
#16197=CARTESIAN_POINT('Ctrl Pts',(90.650315496025,-0.410578522180935,2.16545928159995));
#16198=CARTESIAN_POINT('Ctrl Pts',(90.6517668489606,-0.437060214173424,
2.16027453739834));
#16199=CARTESIAN_POINT('Ctrl Pts',(90.6525075026649,-0.450622925502529,
2.15748619893469));
#16200=CARTESIAN_POINT('Ctrl Pts',(90.6543902654078,-0.485215726762072,
2.15003387790102));
#16201=CARTESIAN_POINT('Ctrl Pts',(90.6555266485398,-0.506205604615391,
2.14518901410195));
#16202=CARTESIAN_POINT('Ctrl Pts',(90.6601228410488,-0.591489096895206,
2.12418247666762));
#16203=CARTESIAN_POINT('Ctrl Pts',(90.6635013051919,-0.655111537125245,
2.10543117425174));
#16204=CARTESIAN_POINT('Ctrl Pts',(90.6736990886196,-0.847902868624687,
2.03902257270528));
#16205=CARTESIAN_POINT('Ctrl Pts',(90.6802701331931,-0.973523772099443,
1.98212107221013));
#16206=CARTESIAN_POINT('Ctrl Pts',(90.6900878577459,-1.14759248575074,1.88271003564006));
#16207=CARTESIAN_POINT('Ctrl Pts',(90.6932003776977,-1.20080476257532,1.84922488380863));
#16208=CARTESIAN_POINT('Ctrl Pts',(90.6982425140115,-1.28206240381173,1.79310397851002));
#16209=CARTESIAN_POINT('Ctrl Pts',(90.7001069248905,-1.31110941621345,1.77197565120365));
#16210=CARTESIAN_POINT('Ctrl Pts',(90.7026401304206,-1.34898454831256,1.74298467995302));
#16211=CARTESIAN_POINT('Ctrl Pts',(90.7032706556186,-1.35828561576675,1.73574626027305));
#16212=CARTESIAN_POINT('Ctrl Pts',(90.7043219638285,-1.37357445775793,1.72364980638154));
#16213=CARTESIAN_POINT('Ctrl Pts',(90.7047398743952,-1.37959569978158,1.71883424084938));
#16214=CARTESIAN_POINT('Ctrl Pts',(90.7055296706781,-1.39086602157835,1.70972328535681));
#16215=CARTESIAN_POINT('Ctrl Pts',(90.7059010528884,-1.39612074071251,1.70543509862382));
#16216=CARTESIAN_POINT('Ctrl Pts',(90.7067892588485,-1.40858398209242,1.69516809648338));
#16217=CARTESIAN_POINT('Ctrl Pts',(90.7073075950979,-1.41577432858068,1.68916747366788));
#16218=CARTESIAN_POINT('Ctrl Pts',(90.7091663352259,-1.44127441965073,1.66760946458652));
#16219=CARTESIAN_POINT('Ctrl Pts',(90.7105231696652,-1.45936714238669,1.65179923960171));
#16220=CARTESIAN_POINT('Ctrl Pts',(90.7223111948723,-1.612499732264,1.51350529212859));
#16221=CARTESIAN_POINT('Ctrl Pts',(90.7335208730586,-1.73211619815348,1.3750012234323));
#16222=CARTESIAN_POINT('Ctrl Pts',(90.7483127503244,-1.87096932705395,1.1669158449815));
#16223=CARTESIAN_POINT('Ctrl Pts',(90.7522658411997,-1.90600311809421,1.10877053820822));
#16224=CARTESIAN_POINT('Ctrl Pts',(90.7587239305597,-1.95994971842568,1.00909941843466));
#16225=CARTESIAN_POINT('Ctrl Pts',(90.7612755175112,-1.98035635047836,0.968438788152192));
#16226=CARTESIAN_POINT('Ctrl Pts',(90.7647905812224,-2.00716980563328,0.91061437450783));
#16227=CARTESIAN_POINT('Ctrl Pts',(90.7657901551802,-2.01464253676964,0.893960091324293));
#16228=CARTESIAN_POINT('Ctrl Pts',(90.7674961362505,-2.02712992069623,0.865177693913809));
#16229=CARTESIAN_POINT('Ctrl Pts',(90.7682059117345,-2.03224464934016,0.853094281436316));
#16230=CARTESIAN_POINT('Ctrl Pts',(90.7696440661534,-2.0424412542888,0.828392863272744));
#16231=CARTESIAN_POINT('Ctrl Pts',(90.7703721421267,-2.04751483784413,0.815772035130639));
#16232=CARTESIAN_POINT('Ctrl Pts',(90.7721981913294,-2.06001226370632,0.783832733050363));
#16233=CARTESIAN_POINT('Ctrl Pts',(90.7732909856817,-2.06728153564264,0.764454950266328));
#16234=CARTESIAN_POINT('Ctrl Pts',(90.777470796035,-2.09425117041366,0.689362059110674));
#16235=CARTESIAN_POINT('Ctrl Pts',(90.7804935068911,-2.11198151125229,0.632963562196727));
#16236=CARTESIAN_POINT('Ctrl Pts',(90.7918592134606,-2.1711293676271,0.414472775958202));
#16237=CARTESIAN_POINT('Ctrl Pts',(90.799732922515,-2.19631362398695,0.248586787085156));
#16238=CARTESIAN_POINT('Ctrl Pts',(90.8116022011743,-2.20524988113747,0.00694075432550717));
#16239=CARTESIAN_POINT('Ctrl Pts',(90.8153291748321,-2.20422236917874,-0.0676543622756929));
#16240=CARTESIAN_POINT('Ctrl Pts',(90.820204932275,-2.19821483892035,-0.160673280659657));
#16241=CARTESIAN_POINT('Ctrl Pts',(90.8211919102693,-2.19677536628233,-0.179282809545848));
#16242=CARTESIAN_POINT('Ctrl Pts',(90.822676060121,-2.19428689507821,-0.206888861870636));
#16243=CARTESIAN_POINT('Ctrl Pts',(90.8231637612441,-2.193418476558,-0.21590127357763));
#16244=CARTESIAN_POINT('Ctrl Pts',(90.8240047594265,-2.1918353102133,-0.231334628047367));
#16245=CARTESIAN_POINT('Ctrl Pts',(90.8243565367105,-2.19114782417496,-0.237758173441339));
#16246=CARTESIAN_POINT('Ctrl Pts',(90.8251686573448,-2.1895030780557,-0.252512546137206));
#16247=CARTESIAN_POINT('Ctrl Pts',(90.8256300500338,-2.18852653273285,-0.260840804905782));
#16248=CARTESIAN_POINT('Ctrl Pts',(90.8269304385665,-2.18565606088373,-0.284169274921833));
#16249=CARTESIAN_POINT('Ctrl Pts',(90.8277750649536,-2.18365530735656,-0.299155588367893));
#16250=CARTESIAN_POINT('Ctrl Pts',(90.8337066694941,-2.16865111886528,-0.40335677729367));
#16251=CARTESIAN_POINT('Ctrl Pts',(90.8390341673297,-2.15033931463097,-0.491713499498828));
#16252=CARTESIAN_POINT('Ctrl Pts',(90.8460251251684,-2.11965781886437,-0.604466953568136));
#16253=CARTESIAN_POINT('Ctrl Pts',(90.847628728038,-2.11217605699912,-0.630112569026625));
#16254=CARTESIAN_POINT('Ctrl Pts',(90.8549531641175,-2.07591641924759,-0.746489627894509));
#16255=CARTESIAN_POINT('Ctrl Pts',(90.8606783571139,-2.04174430628093,-0.835438591472057));
#16256=CARTESIAN_POINT('Ctrl Pts',(90.8697480836424,-1.97722188880606,-0.9755500975986));
#16257=CARTESIAN_POINT('Ctrl Pts',(90.8731693244949,-1.95036905128488,-1.02818567684173));
#16258=CARTESIAN_POINT('Ctrl Pts',(90.8788587876251,-1.90127298599547,-1.11555839638947));
#16259=CARTESIAN_POINT('Ctrl Pts',(90.8811610981769,-1.88011189162641,-1.15086450102903));
#16260=CARTESIAN_POINT('Ctrl Pts',(90.8843889066163,-1.84858353197804,-1.20027482218747));
#16261=CARTESIAN_POINT('Ctrl Pts',(90.8853437065736,-1.83901887259552,-1.21487873247678));
#16262=CARTESIAN_POINT('Ctrl Pts',(90.8869910068826,-1.82210372056902,-1.24004823475346));
#16263=CARTESIAN_POINT('Ctrl Pts',(90.8876864526316,-1.81483241762171,-1.25066578223748));
#16264=CARTESIAN_POINT('Ctrl Pts',(90.8891110388561,-1.7996705880225,-1.27239438292187));
#16265=CARTESIAN_POINT('Ctrl Pts',(90.8898397186364,-1.79176915487626,-1.28349717500584));
#16266=CARTESIAN_POINT('Ctrl Pts',(90.8916982398836,-1.77124429211631,-1.31177897881817));
#16267=CARTESIAN_POINT('Ctrl Pts',(90.8928223010737,-1.75847352556479,-1.32884962806599));
#16268=CARTESIAN_POINT('Ctrl Pts',(90.897390751715,-1.70513258025483,-1.3980344772883));
#16269=CARTESIAN_POINT('Ctrl Pts',(90.9007520663101,-1.662476028188,-1.44849991739415));
#16270=CARTESIAN_POINT('Ctrl Pts',(90.9113478275123,-1.51823294946866,-1.60436720373089));
#16271=CARTESIAN_POINT('Ctrl Pts',(90.918274116129,-1.4084076441104,-1.70159141246577));
#16272=CARTESIAN_POINT('Ctrl Pts',(90.9295646703694,-1.22053561938693,-1.83717063328024));
#16273=CARTESIAN_POINT('Ctrl Pts',(90.9337921035136,-1.14847574208645,-1.88305708896934));
#16274=CARTESIAN_POINT('Ctrl Pts',(90.9392781374331,-1.05664770789302,-1.93429675607218));
#16275=CARTESIAN_POINT('Ctrl Pts',(90.9403234251668,-1.03922245985327,-1.94371421349969));
#16276=CARTESIAN_POINT('Ctrl Pts',(90.9418757017544,-1.01350635399328,-1.95716780680309));
#16277=CARTESIAN_POINT('Ctrl Pts',(90.9423716932234,-1.00531286402195,-1.96138904677404));
#16278=CARTESIAN_POINT('Ctrl Pts',(90.9432206655296,-0.991334661380445,
-1.9684799426538));
#16279=CARTESIAN_POINT('Ctrl Pts',(90.9435720039391,-0.9855634532424,-1.97137575657455));
#16280=CARTESIAN_POINT('Ctrl Pts',(90.9443756280446,-0.972394512590901,
-1.97791124217561));
#16281=CARTESIAN_POINT('Ctrl Pts',(90.9448288771926,-0.964989163385836,
-1.98153472844662));
#16282=CARTESIAN_POINT('Ctrl Pts',(90.9460796873697,-0.94460709583906,-1.99136645848665));
#16283=CARTESIAN_POINT('Ctrl Pts',(90.9468821940927,-0.931589874775223,
-1.99748922909619));
#16284=CARTESIAN_POINT('Ctrl Pts',(90.9514426694677,-0.857885541462968,
-2.03127959817955));
#16285=CARTESIAN_POINT('Ctrl Pts',(90.9553322177099,-0.796031421974158,
-2.05630661342561));
#16286=CARTESIAN_POINT('Ctrl Pts',(90.9672467057016,-0.606435894172123,
-2.12318249433125));
#16287=CARTESIAN_POINT('Ctrl Pts',(90.9754203389746,-0.475905545911,-2.15619679018695));
#16288=CARTESIAN_POINT('Ctrl Pts',(90.9872968001492,-0.27743766252443,-2.18748104812074));
#16289=CARTESIAN_POINT('Ctrl Pts',(90.9911722597462,-0.211259320734743,
-2.19486118639416));
#16290=CARTESIAN_POINT('Ctrl Pts',(90.9975196444823,-0.100062030757739,
-2.20218475922974));
#16291=CARTESIAN_POINT('Ctrl Pts',(91.0000364675163,-0.055198358905565,
-2.20376579462566));
#16292=CARTESIAN_POINT('Ctrl Pts',(91.003510271349,0.0078082011853508,-2.20406068409168));
#16293=CARTESIAN_POINT('Ctrl Pts',(91.0045025148874,0.025932387546345,-2.20392196007757));
#16294=CARTESIAN_POINT('Ctrl Pts',(91.0061978414517,0.057112169692719,-2.20329861913878));
#16295=CARTESIAN_POINT('Ctrl Pts',(91.0069042413448,0.0701687573921278,
-2.2029214604185));
#16296=CARTESIAN_POINT('Ctrl Pts',(91.0082507787625,0.0951775988744194,
-2.20197647102864));
#16297=CARTESIAN_POINT('Ctrl Pts',(91.0088914750374,0.10713005681573,-2.20142733538414));
#16298=CARTESIAN_POINT('Ctrl Pts',(91.0103941129953,0.135282831295993,-2.19990407367748));
#16299=CARTESIAN_POINT('Ctrl Pts',(91.0112534836594,0.15147814608499,-2.19884828214841));
#16300=CARTESIAN_POINT('Ctrl Pts',(91.0142659503734,0.208562368717168,-2.19449320548174));
#16301=CARTESIAN_POINT('Ctrl Pts',(91.0163892343322,0.249370524910688,-2.19023133656061));
#16302=CARTESIAN_POINT('Ctrl Pts',(91.0270571261946,0.456637633807952,-2.1627165156347));
#16303=CARTESIAN_POINT('Ctrl Pts',(91.0350371392582,0.620156215127857,-2.12161940768778));
#16304=CARTESIAN_POINT('Ctrl Pts',(91.0477251057285,0.864146046090899,-2.02964470209689));
#16305=CARTESIAN_POINT('Ctrl Pts',(91.0522951794113,0.948715145275712,-1.99151762594507));
#16306=CARTESIAN_POINT('Ctrl Pts',(91.058200292359,1.0488651162554,-1.9385365037729));
#16307=CARTESIAN_POINT('Ctrl Pts',(91.0592884506128,1.06696810949395,-1.92863184708703));
#16308=CARTESIAN_POINT('Ctrl Pts',(91.060895556087,1.09313346633649,-1.91383491231301));
#16309=CARTESIAN_POINT('Ctrl Pts',(91.0614026145291,1.10130821736325,-1.9091424909212));
#16310=CARTESIAN_POINT('Ctrl Pts',(91.0622990709095,1.11561278366581,-1.90080902412767));
#16311=CARTESIAN_POINT('Ctrl Pts',(91.0626870410073,1.12175539713343,-1.89719046407876));
#16312=CARTESIAN_POINT('Ctrl Pts',(91.0635385486055,1.13513050978949,-1.8892236333736));
#16313=CARTESIAN_POINT('Ctrl Pts',(91.0640028078407,1.14235551495216,-1.88486367776403));
#16314=CARTESIAN_POINT('Ctrl Pts',(91.0653120018854,1.16254812396673,-1.8725196297723));
#16315=CARTESIAN_POINT('Ctrl Pts',(91.0661626198847,1.17545803549536,-1.86444262044296));
#16316=CARTESIAN_POINT('Ctrl Pts',(91.0722839155968,1.2669686416195,-1.80586134344359));
#16317=CARTESIAN_POINT('Ctrl Pts',(91.0778110851321,1.34236502443718,-1.75054209312594));
#16318=CARTESIAN_POINT('Ctrl Pts',(91.0889673667062,1.48536270543473,-1.63093983715516));
#16319=CARTESIAN_POINT('Ctrl Pts',(91.0945841385624,1.55286170479341,-1.56680835157321));
#16320=CARTESIAN_POINT('Ctrl Pts',(91.1067517796543,1.69214083235893,-1.41660852205035));
#16321=CARTESIAN_POINT('Ctrl Pts',(91.1132400255126,1.76183159901642,-1.32893772933579));
#16322=CARTESIAN_POINT('Ctrl Pts',(91.1207978931841,1.8380119167621,-1.21651226797715));
#16323=CARTESIAN_POINT('Ctrl Pts',(91.1221190854593,1.85112643173024,-1.19646182638423));
#16324=CARTESIAN_POINT('Ctrl Pts',(91.1242068108453,1.8715173042875,-1.16414865101554));
#16325=CARTESIAN_POINT('Ctrl Pts',(91.1249811548772,1.87900583413761,-1.15202265194626));
#16326=CARTESIAN_POINT('Ctrl Pts',(91.1264419361295,1.89298804266924,-1.12888250746689));
#16327=CARTESIAN_POINT('Ctrl Pts',(91.1271291881392,1.89950449814457,-1.11788287241177));
#16328=CARTESIAN_POINT('Ctrl Pts',(91.1286889668436,1.91414982215423,-1.09266403616065));
#16329=CARTESIAN_POINT('Ctrl Pts',(91.1295592303648,1.92221669237956,-1.07840959040759));
#16330=CARTESIAN_POINT('Ctrl Pts',(91.1318270318326,1.94295437362976,-1.04079323280673));
#16331=CARTESIAN_POINT('Ctrl Pts',(91.1332153083493,1.95536302511075,-1.01728942309624));
#16332=CARTESIAN_POINT('Ctrl Pts',(91.1450917469282,2.05887571486137,-0.812325678814625));
#16333=CARTESIAN_POINT('Ctrl Pts',(91.1546202630543,2.12491977230903,-0.619320684074938));
#16334=CARTESIAN_POINT('Ctrl Pts',(91.1674443760715,2.17487539091969,-0.361975956396143));
#16335=CARTESIAN_POINT('Ctrl Pts',(91.1703735351449,2.18379959145835,-0.303526171115663));
#16336=CARTESIAN_POINT('Ctrl Pts',(91.1751521196547,2.19419072316193,-0.210547809353404));
#16337=CARTESIAN_POINT('Ctrl Pts',(91.1769419170975,2.1972140151268,-0.176220397250195));
#16338=CARTESIAN_POINT('Ctrl Pts',(91.1793810230299,2.20016862701943,-0.130404325849278));
#16339=CARTESIAN_POINT('Ctrl Pts',(91.1799941767993,2.20081679071618,-0.118965195789882));
#16340=CARTESIAN_POINT('Ctrl Pts',(91.181017919216,2.20174267312989,-0.100008896740413));
#16341=CARTESIAN_POINT('Ctrl Pts',(91.1814257407627,2.20207115751675,-0.0924942825992905));
#16342=CARTESIAN_POINT('Ctrl Pts',(91.1822008422639,2.20261938775447,-0.0782859268993837));
#16343=CARTESIAN_POINT('Ctrl Pts',(91.1825676591037,2.20284710209822,-0.0715925691408228));
#16344=CARTESIAN_POINT('Ctrl Pts',(91.1834452175826,2.20331676375726,-0.0556494040281865));
#16345=CARTESIAN_POINT('Ctrl Pts',(91.1839574520496,2.20353097234369,-0.0463989798159462));
#16346=CARTESIAN_POINT('Ctrl Pts',(91.1855246181047,2.20400538663348,-0.0182555968829399));
#16347=CARTESIAN_POINT('Ctrl Pts',(91.1865887633008,2.2040808866569,0.000639150944144555));
#16348=CARTESIAN_POINT('Ctrl Pts',(91.1939716982295,2.202930395477,0.130456778283692));
#16349=CARTESIAN_POINT('Ctrl Pts',(91.2006180440115,2.19357438941952,0.241140712553303));
#16350=CARTESIAN_POINT('Ctrl Pts',(91.2134217847883,2.15966681699686,0.451557317539482));
#16351=CARTESIAN_POINT('Ctrl Pts',(91.2195612596613,2.13640254015311,0.551227138726623));
#16352=CARTESIAN_POINT('Ctrl Pts',(91.2302309579572,2.08269194356501,0.725562396785453));
#16353=CARTESIAN_POINT('Ctrl Pts',(91.2348167695877,2.0549147549709,0.800858362059234));
#16354=CARTESIAN_POINT('Ctrl Pts',(91.2404910108436,2.01434811643794,0.894708518273887));
#16355=CARTESIAN_POINT('Ctrl Pts',(91.241703818383,2.00530104858002,0.914805674071664));
#16356=CARTESIAN_POINT('Ctrl Pts',(91.2436608237272,1.99008890385953,0.947287379801753));
#16357=CARTESIAN_POINT('Ctrl Pts',(91.2444112336959,1.98410615045209,0.959755188154415));
#16358=CARTESIAN_POINT('Ctrl Pts',(91.2458528865144,1.97232365401225,0.983728307146277));
#16359=CARTESIAN_POINT('Ctrl Pts',(91.2465446382939,1.96653960351286,0.995240662371494));
#16360=CARTESIAN_POINT('Ctrl Pts',(91.2481363840608,1.95292968726279,1.02174736777968));
#16361=CARTESIAN_POINT('Ctrl Pts',(91.2490337878753,1.94503145297032,1.0367037741863));
#16362=CARTESIAN_POINT('Ctrl Pts',(91.2519634877876,1.91851244514409,1.08555111325186));
#16363=CARTESIAN_POINT('Ctrl Pts',(91.2539702043777,1.89917142430908,1.1190439482456));
#16364=CARTESIAN_POINT('Ctrl Pts',(91.264761568948,1.78896361845481,1.29879545029872));
#16365=CARTESIAN_POINT('Ctrl Pts',(91.2729318478896,1.68208320932294,1.43452394000362));
#16366=CARTESIAN_POINT('Ctrl Pts',(91.2858770212533,1.49398320987748,1.62311417647994));
#16367=CARTESIAN_POINT('Ctrl Pts',(91.2905137884267,1.42327640239945,1.68545734946492));
#16368=CARTESIAN_POINT('Ctrl Pts',(91.296501040871,1.33238898008588,1.75578660022845));
#16369=CARTESIAN_POINT('Ctrl Pts',(91.297595493826,1.31579233430909,1.76825831008208));
#16370=CARTESIAN_POINT('Ctrl Pts',(91.2992090931374,1.29140764741413,1.78604903129823));
#16371=CARTESIAN_POINT('Ctrl Pts',(91.2997161207993,1.28375727116081,1.79155578092814));
#16372=CARTESIAN_POINT('Ctrl Pts',(91.3006150435772,1.27022114846199,1.80116787872404));
#16373=CARTESIAN_POINT('Ctrl Pts',(91.3010055317506,1.26435034358085,1.8052937989297));
#16374=CARTESIAN_POINT('Ctrl Pts',(91.3018589264266,1.25154155048389,1.81420251155795));
#16375=CARTESIAN_POINT('Ctrl Pts',(91.3023225224186,1.24459634837588,1.81897414228444));
#16376=CARTESIAN_POINT('Ctrl Pts',(91.3036293407401,1.22504901590938,1.83223957684663));
#16377=CARTESIAN_POINT('Ctrl Pts',(91.3044782265253,1.21238638024956,1.84064287605444));
#16378=CARTESIAN_POINT('Ctrl Pts',(91.3105155569658,1.12248686899113,1.89897272355935));
#16379=CARTESIAN_POINT('Ctrl Pts',(91.3159529098435,1.04228466027102,1.94414858320991));
#16380=CARTESIAN_POINT('Ctrl Pts',(91.3227377034689,0.940192452085248,1.99351807562356));
#16381=CARTESIAN_POINT('Ctrl Pts',(91.3240244647457,0.920745314560739,2.00257439783287));
#16382=CARTESIAN_POINT('Ctrl Pts',(91.3305826079087,0.821072309124219,2.04723219089107));
#16383=CARTESIAN_POINT('Ctrl Pts',(91.3358644292024,0.738900107659062,2.07830390606254));
#16384=CARTESIAN_POINT('Ctrl Pts',(91.3449146092867,0.592604151018397,2.12384542922043));
#16385=CARTESIAN_POINT('Ctrl Pts',(91.3487228091861,0.52927763251353,2.14050586583685));
#16386=CARTESIAN_POINT('Ctrl Pts',(91.3549731701778,0.421965731992394,2.16368350628457));
#16387=CARTESIAN_POINT('Ctrl Pts',(91.3574585433306,0.378357675664242,2.17173369960022));
#16388=CARTESIAN_POINT('Ctrl Pts',(91.3608961712463,0.316719760133843,2.18119908054758));
#16389=CARTESIAN_POINT('Ctrl Pts',(91.3618827938221,0.298872150271845,2.1837161675648));
#16390=CARTESIAN_POINT('Ctrl Pts',(91.3635706694203,0.268073668796116,2.18767507532186));
#16391=CARTESIAN_POINT('Ctrl Pts',(91.3642751863364,0.255137388358216,2.18922147128726));
#16392=CARTESIAN_POINT('Ctrl Pts',(91.3656195439144,0.230300400161042,2.19196732798056));
#16393=CARTESIAN_POINT('Ctrl Pts',(91.3662599281512,0.21840218464924,2.19318479265922));
#16394=CARTESIAN_POINT('Ctrl Pts',(91.3679311333082,0.18718022466682,2.19612292635137));
#16395=CARTESIAN_POINT('Ctrl Pts',(91.3689569700343,0.167842418419153,2.19768544127829));
#16396=CARTESIAN_POINT('Ctrl Pts',(91.3725748857664,0.0990632065834146,
2.2023297297749));
#16397=CARTESIAN_POINT('Ctrl Pts',(91.3751232243473,0.0495399332369143,
2.204));
#16398=CARTESIAN_POINT('Ctrl Pts',(91.3776298668357,4.55134372080087E-12,
2.204));
#16399=CARTESIAN_POINT('Origin',(66.9212607628943,0.,0.));
#16400=CARTESIAN_POINT('',(92.2356508702176,-2.51612300885953E-11,2.204));
#16401=CARTESIAN_POINT('',(92.1243308360554,1.24847509279933E-11,2.204));
#16402=CARTESIAN_POINT('',(66.9212607628943,-2.69912154532077E-16,2.204));
#16403=CARTESIAN_POINT('Ctrl Pts',(92.2356508702176,-2.51603599066286E-11,
2.204));
#16404=CARTESIAN_POINT('Ctrl Pts',(92.2292589034109,0.108362820276164,2.20400000000124));
#16405=CARTESIAN_POINT('Ctrl Pts',(92.2226946757361,0.216577546288409,2.1960083774407));
#16406=CARTESIAN_POINT('Ctrl Pts',(92.2094793534317,0.435170017473937,2.16354518765205));
#16407=CARTESIAN_POINT('Ctrl Pts',(92.2028565183254,0.545153221931167,2.13848404676721));
#16408=CARTESIAN_POINT('Ctrl Pts',(92.1943936693437,0.688154827320078,2.09414254451766));
#16409=CARTESIAN_POINT('Ctrl Pts',(92.1923261000641,0.723278957464229,2.08227227989087));
#16410=CARTESIAN_POINT('Ctrl Pts',(92.1893675102199,0.773796971725582,2.06376697137654));
#16411=CARTESIAN_POINT('Ctrl Pts',(92.1884535116523,0.789439680567183,2.05783402589375));
#16412=CARTESIAN_POINT('Ctrl Pts',(92.1868552427004,0.816851609794035,2.04707868898289));
#16413=CARTESIAN_POINT('Ctrl Pts',(92.1861684893062,0.828649332558261,2.04233151188323));
#16414=CARTESIAN_POINT('Ctrl Pts',(92.1847417837419,0.853194852320118,2.03220715978855));
#16415=CARTESIAN_POINT('Ctrl Pts',(92.1840024937463,0.86593446000815,2.02681151547419));
#16416=CARTESIAN_POINT('Ctrl Pts',(92.1820737400488,0.899217268331408,2.01234405222682));
#16417=CARTESIAN_POINT('Ctrl Pts',(92.1808909526023,0.91967436673315,2.00307747940364));
#16418=CARTESIAN_POINT('Ctrl Pts',(92.1756329291041,1.01075067475344,1.96013263798239));
#16419=CARTESIAN_POINT('Ctrl Pts',(92.171676844361,1.07969131529775,1.92301980081122));
#16420=CARTESIAN_POINT('Ctrl Pts',(92.160912793194,1.26534000614474,1.80994133437855));
#16421=CARTESIAN_POINT('Ctrl Pts',(92.1543210805396,1.37703898871843,1.72648073941178));
#16422=CARTESIAN_POINT('Ctrl Pts',(92.1446812081425,1.52289466453686,1.5942835031326));
#16423=CARTESIAN_POINT('Ctrl Pts',(92.1418167677432,1.56412337990898,1.55385500366132));
#16424=CARTESIAN_POINT('Ctrl Pts',(92.1371358196637,1.62693705320157,1.48722487716522));
#16425=CARTESIAN_POINT('Ctrl Pts',(92.135376279173,1.64958691752246,1.46206182181309));
#16426=CARTESIAN_POINT('Ctrl Pts',(92.1329761841985,1.67902122393059,1.42780662433645));
#16427=CARTESIAN_POINT('Ctrl Pts',(92.132370540746,1.68632900262063,1.41916824612901));
#16428=CARTESIAN_POINT('Ctrl Pts',(92.1313587542599,1.69833158737897,1.40475662815667));
#16429=CARTESIAN_POINT('Ctrl Pts',(92.1309553043602,1.70306434595517,1.39901508063903));
#16430=CARTESIAN_POINT('Ctrl Pts',(92.1301880209674,1.71196211357715,1.38810869304045));
#16431=CARTESIAN_POINT('Ctrl Pts',(92.1298246374551,1.71613305115042,1.38294879527531));
#16432=CARTESIAN_POINT('Ctrl Pts',(92.1289552396416,1.72601196449929,1.37061400787798));
#16433=CARTESIAN_POINT('Ctrl Pts',(92.1284477592989,1.73169854804443,1.36342223571383));
#16434=CARTESIAN_POINT('Ctrl Pts',(92.126895317366,1.7488591753901,1.34143879155896));
#16435=CARTESIAN_POINT('Ctrl Pts',(92.1258413065812,1.76018950935915,1.32653657754112));
#16436=CARTESIAN_POINT('Ctrl Pts',(92.1186229649665,1.83574515312804,1.22448958767468));
#16437=CARTESIAN_POINT('Ctrl Pts',(92.1121455582501,1.8936595333111,1.13286577251837));
#16438=CARTESIAN_POINT('Ctrl Pts',(92.1000412918268,1.98851628772828,0.955051401001784));
#16439=CARTESIAN_POINT('Ctrl Pts',(92.0944317401465,2.02715958570171,0.870026308189507));
#16440=CARTESIAN_POINT('Ctrl Pts',(92.0836015185267,2.09254246197751,0.697942251155415));
#16441=CARTESIAN_POINT('Ctrl Pts',(92.0783846279476,2.11951464828223,0.611161350368453));
#16442=CARTESIAN_POINT('Ctrl Pts',(92.0720806754785,2.1464399985641,0.500924758781559));
#16443=CARTESIAN_POINT('Ctrl Pts',(92.0708316928622,2.15148067542277,0.478812321252053));
#16444=CARTESIAN_POINT('Ctrl Pts',(92.0688357689462,2.15905543247835,0.443044416788347));
#16445=CARTESIAN_POINT('Ctrl Pts',(92.0680820477926,2.16180322093066,0.429436330706117));
#16446=CARTESIAN_POINT('Ctrl Pts',(92.0666465314981,2.16681869998734,0.403328737558804));
#16447=CARTESIAN_POINT('Ctrl Pts',(92.0659640967017,2.16910724988882,0.390833848325662));
#16448=CARTESIAN_POINT('Ctrl Pts',(92.0644112576972,2.17409357221107,0.362215881542153));
#16449=CARTESIAN_POINT('Ctrl Pts',(92.0635431384464,2.17672026521733,0.346081077212601));
#16450=CARTESIAN_POINT('Ctrl Pts',(92.0612352638749,2.18326713039083,0.302837896303151));
#16451=CARTESIAN_POINT('Ctrl Pts',(92.0598057103574,2.18686196569118,0.275682758105604));
#16452=CARTESIAN_POINT('Ctrl Pts',(92.0499334775996,2.20840374751872,0.0858167061214575));
#16453=CARTESIAN_POINT('Ctrl Pts',(92.0420747003095,2.2086812416632,-0.0783817608894441));
#16454=CARTESIAN_POINT('Ctrl Pts',(92.0282231437749,2.17736107979107,-0.362965310556047));
#16455=CARTESIAN_POINT('Ctrl Pts',(92.0222638896055,2.15380762064295,-0.483477909052407));
#16456=CARTESIAN_POINT('Ctrl Pts',(92.0149784920738,2.11598575199715,-0.61682879972263));
#16457=CARTESIAN_POINT('Ctrl Pts',(92.0141269470507,2.11143908377422,-0.632217080300995));
#16458=CARTESIAN_POINT('Ctrl Pts',(92.0128121395605,2.10423867246123,-0.65564259924182));
#16459=CARTESIAN_POINT('Ctrl Pts',(92.0123555776976,2.10170588799374,-0.663716780081136));
#16460=CARTESIAN_POINT('Ctrl Pts',(92.0115113391599,2.096964992006,-0.67853085626438));
#16461=CARTESIAN_POINT('Ctrl Pts',(92.0111244620461,2.09477077347478,-0.685274910586024));
#16462=CARTESIAN_POINT('Ctrl Pts',(92.0102335584211,2.08966828156304,-0.700704190102408));
#16463=CARTESIAN_POINT('Ctrl Pts',(92.0097283035788,2.08673839860801,-0.709381941296212));
#16464=CARTESIAN_POINT('Ctrl Pts',(92.0081337137861,2.0773757097611,-0.736552458233469));
#16465=CARTESIAN_POINT('Ctrl Pts',(92.0070339834833,2.07075068137228,-0.754977433310458));
#16466=CARTESIAN_POINT('Ctrl Pts',(91.9978763183944,2.01412939086529,-0.906093372363755));
#16467=CARTESIAN_POINT('Ctrl Pts',(91.9892797493675,1.9516830603304,-1.03375560521944));
#16468=CARTESIAN_POINT('Ctrl Pts',(91.9719287786869,1.80015599103027,-1.28015889349355));
#16469=CARTESIAN_POINT('Ctrl Pts',(91.9632346386924,1.71047172036522,-1.39773653445652));
#16470=CARTESIAN_POINT('Ctrl Pts',(91.9535974999737,1.59240899594199,-1.52397187950321));
#16471=CARTESIAN_POINT('Ctrl Pts',(91.9521995715264,1.57480144341366,-1.54215991036318));
#16472=CARTESIAN_POINT('Ctrl Pts',(91.950025178691,1.54665866402641,-1.57024573459299));
#16473=CARTESIAN_POINT('Ctrl Pts',(91.9492396097857,1.53633313498483,-1.58034970887763));
#16474=CARTESIAN_POINT('Ctrl Pts',(91.9477772905553,1.5168183141829,-1.59907376797166));
#16475=CARTESIAN_POINT('Ctrl Pts',(91.9470995045348,1.50765305028828,-1.60771794876071));
#16476=CARTESIAN_POINT('Ctrl Pts',(91.9455869056911,1.48693203595516,-1.62692786125148));
#16477=CARTESIAN_POINT('Ctrl Pts',(91.9447539650389,1.47533673800317,-1.63745005173476));
#16478=CARTESIAN_POINT('Ctrl Pts',(91.9423267201468,1.44101343100652,-1.66793625292117));
#16479=CARTESIAN_POINT('Ctrl Pts',(91.9407466139509,1.41798494050082,-1.68755736994441));
#16480=CARTESIAN_POINT('Ctrl Pts',(91.9308945197218,1.2702782197703,-1.8082498664395));
#16481=CARTESIAN_POINT('Ctrl Pts',(91.9231771740635,1.13527811194518,-1.89592270148551));
#16482=CARTESIAN_POINT('Ctrl Pts',(91.9093122623397,0.879278297752528,-2.02494530864642));
#16483=CARTESIAN_POINT('Ctrl Pts',(91.903190707613,0.761957750317959,-2.07194273594277));
#16484=CARTESIAN_POINT('Ctrl Pts',(91.8957338898569,0.62634517940553,-2.11318512218995));
#16485=CARTESIAN_POINT('Ctrl Pts',(91.8949049601088,0.611363991790129,-2.11756787057247));
#16486=CARTESIAN_POINT('Ctrl Pts',(91.8936179581179,0.588279148973086,-2.12405595903169));
#16487=CARTESIAN_POINT('Ctrl Pts',(91.8931661562179,0.580207649863388,-2.12627494754705));
#16488=CARTESIAN_POINT('Ctrl Pts',(91.8923260822335,0.565265101118912,-2.13029148397796));
#16489=CARTESIAN_POINT('Ctrl Pts',(91.8919385459556,0.558397779714571,-2.13210186351864));
#16490=CARTESIAN_POINT('Ctrl Pts',(91.8910484528981,0.542682716396138,-2.13616357488154));
#16491=CARTESIAN_POINT('Ctrl Pts',(91.8905446920729,0.533829642173803,-2.13839314822935));
#16492=CARTESIAN_POINT('Ctrl Pts',(91.8889309677394,0.505590079216,-2.14531875496729));
#16493=CARTESIAN_POINT('Ctrl Pts',(91.8878101031735,0.486154098329247,-2.14980650858141));
#16494=CARTESIAN_POINT('Ctrl Pts',(91.8789429092045,0.333527782278194,-2.18287229632642));
#16495=CARTESIAN_POINT('Ctrl Pts',(91.8707011945206,0.198017004896817,-2.19930821391621));
#16496=CARTESIAN_POINT('Ctrl Pts',(91.8533571707245,-0.0908354350552137,
-2.2074196346521));
#16497=CARTESIAN_POINT('Ctrl Pts',(91.8443338211819,-0.243592257073614,
-2.19582084869509));
#16498=CARTESIAN_POINT('Ctrl Pts',(91.8344122704404,-0.418702875786694,
-2.16400955307388));
#16499=CARTESIAN_POINT('Ctrl Pts',(91.8330224797841,-0.44338770236666,-2.15908704399322));
#16500=CARTESIAN_POINT('Ctrl Pts',(91.8308578082635,-0.482070479621216,
-2.15068172066911));
#16501=CARTESIAN_POINT('Ctrl Pts',(91.8300739570427,-0.496127269191218,
-2.14748260938351));
#16502=CARTESIAN_POINT('Ctrl Pts',(91.8286132032865,-0.522411149182497,
-2.14122894343726));
#16503=CARTESIAN_POINT('Ctrl Pts',(91.8279352855326,-0.534645328525603,
-2.13820700093575));
#16504=CARTESIAN_POINT('Ctrl Pts',(91.8264203050548,-0.562062407453119,
-2.13118472882097));
#16505=CARTESIAN_POINT('Ctrl Pts',(91.8255851415365,-0.577229915056059,
-2.12712673357661));
#16506=CARTESIAN_POINT('Ctrl Pts',(91.8231448807168,-0.621690001683358,
-2.11472107088538));
#16507=CARTESIAN_POINT('Ctrl Pts',(91.8215542183305,-0.650854992629008,
-2.1059277202488));
#16508=CARTESIAN_POINT('Ctrl Pts',(91.8118917641264,-0.828852541915464,
-2.04820957818735));
#16509=CARTESIAN_POINT('Ctrl Pts',(91.8043442148215,-0.972299366408334,
-1.98413656711356));
#16510=CARTESIAN_POINT('Ctrl Pts',(91.7923917254874,-1.1860195688343,-1.859884515572));
#16511=CARTESIAN_POINT('Ctrl Pts',(91.7880061887851,-1.26140689016486,-1.80960315733449));
#16512=CARTESIAN_POINT('Ctrl Pts',(91.7811757802579,-1.36913612883749,-1.72774052240596));
#16513=CARTESIAN_POINT('Ctrl Pts',(91.7788712435987,-1.40395221871258,-1.6995701519728));
#16514=CARTESIAN_POINT('Ctrl Pts',(91.7758388653087,-1.44732806862101,-1.66223125549688));
#16515=CARTESIAN_POINT('Ctrl Pts',(91.7751734453719,-1.45670289370946,-1.65402175014187));
#16516=CARTESIAN_POINT('Ctrl Pts',(91.774088162018,-1.47174943637311,-1.64061839890208));
#16517=CARTESIAN_POINT('Ctrl Pts',(91.7736718343597,-1.47746459512303,-1.63547347906882));
#16518=CARTESIAN_POINT('Ctrl Pts',(91.7728592083842,-1.48850646148873,-1.62542822068468));
#16519=CARTESIAN_POINT('Ctrl Pts',(91.772463162685,-1.49383613424061,-1.62053138984471));
#16520=CARTESIAN_POINT('Ctrl Pts',(91.771572404995,-1.50571056742104,-1.60951296847784));
#16521=CARTESIAN_POINT('Ctrl Pts',(91.7710766691195,-1.51224230741066,-1.60337753088721));
#16522=CARTESIAN_POINT('Ctrl Pts',(91.7693205534058,-1.53511968954436,-1.5816240521812));
#16523=CARTESIAN_POINT('Ctrl Pts',(91.7680454757852,-1.55126174648873,-1.56579501107886));
#16524=CARTESIAN_POINT('Ctrl Pts',(91.7583708394835,-1.67052427240142,-1.44519068003146));
#16525=CARTESIAN_POINT('Ctrl Pts',(91.7494286567537,-1.76316839327559,-1.3305865807152));
#16526=CARTESIAN_POINT('Ctrl Pts',(91.7350743865384,-1.89452473885927,-1.13004107430255));
#16527=CARTESIAN_POINT('Ctrl Pts',(91.7295852564873,-1.94039567161276,-1.04932552983398));
#16528=CARTESIAN_POINT('Ctrl Pts',(91.7210390426506,-2.00553903071472,-0.915724834337237));
#16529=CARTESIAN_POINT('Ctrl Pts',(91.717884313861,-2.02811272669317,-0.864579857683288));
#16530=CARTESIAN_POINT('Ctrl Pts',(91.7137174048247,-2.05590711753306,-0.794507374510997));
#16531=CARTESIAN_POINT('Ctrl Pts',(91.7126478713954,-2.06285435441513,-0.776291176720659));
#16532=CARTESIAN_POINT('Ctrl Pts',(91.710867143915,-2.0741024470485,-0.745580015018834));
#16533=CARTESIAN_POINT('Ctrl Pts',(91.7101516181694,-2.07853418902356,-0.733134472906203));
#16534=CARTESIAN_POINT('Ctrl Pts',(91.7087450225014,-2.08707004861234,-0.708463749710086));
#16535=CARTESIAN_POINT('Ctrl Pts',(91.708053805019,-2.09117930068661,-0.696240917068855));
#16536=CARTESIAN_POINT('Ctrl Pts',(91.706376830118,-2.10093754151623,-0.666349391221354));
#16537=CARTESIAN_POINT('Ctrl Pts',(91.705394886591,-2.10647125442536,-0.64864392925449));
#16538=CARTESIAN_POINT('Ctrl Pts',(91.7020397650123,-2.12474419601195,-0.587476924950216));
#16539=CARTESIAN_POINT('Ctrl Pts',(91.6997025681194,-2.13636743309628,-0.543692553489345));
#16540=CARTESIAN_POINT('Ctrl Pts',(91.6890375462149,-2.18394678824568,-0.339249517722378));
#16541=CARTESIAN_POINT('Ctrl Pts',(91.681230242233,-2.20318018519569,-0.175249667298765));
#16542=CARTESIAN_POINT('Ctrl Pts',(91.6687584183441,-2.20441683530105,0.0810862893957523));
#16543=CARTESIAN_POINT('Ctrl Pts',(91.6642336862404,-2.1991334509297,0.172735538709611));
#16544=CARTESIAN_POINT('Ctrl Pts',(91.6583875930756,-2.18571214328869,0.284070644352944));
#16545=CARTESIAN_POINT('Ctrl Pts',(91.6573096193201,-2.182984064873,0.304325841682489));
#16546=CARTESIAN_POINT('Ctrl Pts',(91.6557186660863,-2.17860284762251,0.333755063207317));
#16547=CARTESIAN_POINT('Ctrl Pts',(91.6552174113932,-2.17717249237597,0.342961720874635));
#16548=CARTESIAN_POINT('Ctrl Pts',(91.6543281377425,-2.17454858312275,0.359172577760697));
#16549=CARTESIAN_POINT('Ctrl Pts',(91.6539414867107,-2.1733794756698,0.366180466757193));
#16550=CARTESIAN_POINT('Ctrl Pts',(91.6530962613843,-2.17076298476524,0.381410215844643));
#16551=CARTESIAN_POINT('Ctrl Pts',(91.6526370079661,-2.16930279018705,0.389629424653586));
#16552=CARTESIAN_POINT('Ctrl Pts',(91.6513417375729,-2.16507581827842,0.412661831270366));
#16553=CARTESIAN_POINT('Ctrl Pts',(91.6505001434403,-2.16220380953962,0.427454964131804));
#16554=CARTESIAN_POINT('Ctrl Pts',(91.6445678690501,-2.14107132115198,0.530636996928126));
#16555=CARTESIAN_POINT('Ctrl Pts',(91.6392369060706,-2.11754959161597,0.61785331576506));
#16556=CARTESIAN_POINT('Ctrl Pts',(91.6324450230468,-2.08130342556231,0.725490664067775));
#16557=CARTESIAN_POINT('Ctrl Pts',(91.6310452373882,-2.07350474498486,0.747488267342352));
#16558=CARTESIAN_POINT('Ctrl Pts',(91.62434902203,-2.03457634320534,0.851992448161574));
#16559=CARTESIAN_POINT('Ctrl Pts',(91.6190423037823,-1.99886162223261,0.932708625779653));
#16560=CARTESIAN_POINT('Ctrl Pts',(91.609975893247,-1.9284351121572,1.06912222443641));
#16561=CARTESIAN_POINT('Ctrl Pts',(91.6061750239318,-1.89589627490835,1.1258164640384));
#16562=CARTESIAN_POINT('Ctrl Pts',(91.5999399614086,-1.8372014427085,1.21830222802047));
#16563=CARTESIAN_POINT('Ctrl Pts',(91.5974625496646,-1.81240030819396,1.25490038556612));
#16564=CARTESIAN_POINT('Ctrl Pts',(91.594039917803,-1.77603503738983,1.30523397244636));
#16565=CARTESIAN_POINT('Ctrl Pts',(91.5930604675904,-1.76537961357666,1.31961017861556));
#16566=CARTESIAN_POINT('Ctrl Pts',(91.5913864298554,-1.74674069004093,1.34412777336433));
#16567=CARTESIAN_POINT('Ctrl Pts',(91.5906886072256,-1.73884113575029,1.35433157827334));
#16568=CARTESIAN_POINT('Ctrl Pts',(91.5893581876538,-1.72353268344536,1.3737506610727));
#16569=CARTESIAN_POINT('Ctrl Pts',(91.5887250454644,-1.71613837163128,1.38297682070981));
#16570=CARTESIAN_POINT('Ctrl Pts',(91.5870756340192,-1.69659182655424,1.40696759812028));
#16571=CARTESIAN_POINT('Ctrl Pts',(91.5860641919308,-1.68432092249591,1.42163452015283));
#16572=CARTESIAN_POINT('Ctrl Pts',(91.5824965827552,-1.64004350379028,1.47317939291205));
#16573=CARTESIAN_POINT('Ctrl Pts',(91.579982947469,-1.607003189443,1.50915254989417));
#16574=CARTESIAN_POINT('Ctrl Pts',(91.5693511268562,-1.45992062750809,1.65897797078968));
#16575=CARTESIAN_POINT('Ctrl Pts',(91.5617111185671,-1.3347844079203,1.76122910246705));
#16576=CARTESIAN_POINT('Ctrl Pts',(91.5494617479465,-1.12367950143193,1.8981976602712));
#16577=CARTESIAN_POINT('Ctrl Pts',(91.5449922625519,-1.04478538648991,1.94273788818145));
#16578=CARTESIAN_POINT('Ctrl Pts',(91.5392138171219,-0.94511276301666,1.99117819444384));
#16579=CARTESIAN_POINT('Ctrl Pts',(91.5381421039575,-0.926719158480925,
1.99980506055949));
#16580=CARTESIAN_POINT('Ctrl Pts',(91.5365587222451,-0.899740337264539,
2.01200639279583));
#16581=CARTESIAN_POINT('Ctrl Pts',(91.5360586214673,-0.891247095780816,
2.01578297619448));
#16582=CARTESIAN_POINT('Ctrl Pts',(91.5351705895025,-0.876221705145017,
2.02235060758127));
#16583=CARTESIAN_POINT('Ctrl Pts',(91.5347840116903,-0.869699594866195,
2.02516396119144));
#16584=CARTESIAN_POINT('Ctrl Pts',(91.5339379629519,-0.855467938706829,
2.03122144589011));
#16585=CARTESIAN_POINT('Ctrl Pts',(91.5334778018349,-0.847753600945764,
2.03445319035581));
#16586=CARTESIAN_POINT('Ctrl Pts',(91.5321776610022,-0.826024083013494,
2.04341122389381));
#16587=CARTESIAN_POINT('Ctrl Pts',(91.5313320410067,-0.811968283577297,
2.04903701680671));
#16588=CARTESIAN_POINT('Ctrl Pts',(91.525135540866,-0.70942853099964,2.0888575419592));
#16589=CARTESIAN_POINT('Ctrl Pts',(91.5195195484463,-0.618884030880044,
2.11744984807348));
#16590=CARTESIAN_POINT('Ctrl Pts',(91.5124900591962,-0.504872575052794,
2.14551372293018));
#16591=CARTESIAN_POINT('Ctrl Pts',(91.5111353931813,-0.482874269982661,
2.15057152408412));
#16592=CARTESIAN_POINT('Ctrl Pts',(91.5040061829274,-0.366801161465693,
2.17538801856326));
#16593=CARTESIAN_POINT('Ctrl Pts',(91.498227930365,-0.271581082322755,2.18931533262676));
#16594=CARTESIAN_POINT('Ctrl Pts',(91.4891595822157,-0.117678594080809,
2.2016271017));
#16595=CARTESIAN_POINT('Ctrl Pts',(91.4857881136124,-0.059440386435164,
2.20396864495139));
#16596=CARTESIAN_POINT('Ctrl Pts',(91.4824602988302,-0.000782819936893213,
2.20399989587492));
#16597=CARTESIAN_POINT('Ctrl Pts',(91.4824380960676,-0.000391409701139083,
2.204));
#16598=CARTESIAN_POINT('Ctrl Pts',(91.4824158962551,-3.3646198792706E-12,
2.204));
#16599=CARTESIAN_POINT('Ctrl Pts',(91.3776298668357,4.55134372080087E-12,
2.204));
#16600=CARTESIAN_POINT('Ctrl Pts',(91.3776497873187,-0.000393697700173932,
2.204));
#16601=CARTESIAN_POINT('Ctrl Pts',(91.3776697052255,-0.0007873964541778,
2.20399989455858));
#16602=CARTESIAN_POINT('Ctrl Pts',(91.3817409009304,-0.0812697516293409,
2.20395676479764));
#16603=CARTESIAN_POINT('Ctrl Pts',(91.3856766082689,-0.161299799345881,
2.19954852774969));
#16604=CARTESIAN_POINT('Ctrl Pts',(91.3950873875084,-0.353788069461133,
2.17838110266901));
#16605=CARTESIAN_POINT('Ctrl Pts',(91.4005006362243,-0.465527647417681,
2.15726502739082));
#16606=CARTESIAN_POINT('Ctrl Pts',(91.4063620569227,-0.579759015343803,
2.12638622936986));
#16607=CARTESIAN_POINT('Ctrl Pts',(91.4065995345294,-0.584375747435629,
2.12512209008459));
#16608=CARTESIAN_POINT('Ctrl Pts',(91.4098781767823,-0.647949740735055,
2.10749162497104));
#16609=CARTESIAN_POINT('Ctrl Pts',(91.412982708196,-0.706200208886684,2.08869334756884));
#16610=CARTESIAN_POINT('Ctrl Pts',(91.4169634216333,-0.77697600000046,2.06255375000772));
#16611=CARTESIAN_POINT('Ctrl Pts',(91.417723017175,-0.790314941408937,2.05747951346729));
#16612=CARTESIAN_POINT('Ctrl Pts',(91.4189273759722,-0.811180928265386,
2.04930908499334));
#16613=CARTESIAN_POINT('Ctrl Pts',(91.419367140723,-0.818741929583332,2.04630004462266));
#16614=CARTESIAN_POINT('Ctrl Pts',(91.4202030750725,-0.832999891793393,
2.04053415280962));
#16615=CARTESIAN_POINT('Ctrl Pts',(91.4205987319439,-0.839700135165113,
2.03778608444771));
#16616=CARTESIAN_POINT('Ctrl Pts',(91.4215420333139,-0.855562941688378,
2.03118852495752));
#16617=CARTESIAN_POINT('Ctrl Pts',(91.4220913818566,-0.864713170045411,
2.02731001499579));
#16618=CARTESIAN_POINT('Ctrl Pts',(91.4239617528901,-0.895585130120537,
2.0139772814237));
#16619=CARTESIAN_POINT('Ctrl Pts',(91.4252985594738,-0.917179859359909,
2.00423507311758));
#16620=CARTESIAN_POINT('Ctrl Pts',(91.4286290665147,-0.969961077375128,
1.97939181664637));
#16621=CARTESIAN_POINT('Ctrl Pts',(91.4306400661709,-1.00095603528033,1.96390001061502));
#16622=CARTESIAN_POINT('Ctrl Pts',(91.4395640170308,-1.13532990018562,1.89273025986807));
#16623=CARTESIAN_POINT('Ctrl Pts',(91.4466850750587,-1.23452874148243,1.8295736791617));
#16624=CARTESIAN_POINT('Ctrl Pts',(91.4615790492524,-1.43330479531993,1.67946206313205));
#16625=CARTESIAN_POINT('Ctrl Pts',(91.4692890590268,-1.53107594060421,1.59083972993484));
#16626=CARTESIAN_POINT('Ctrl Pts',(91.4780066811962,-1.63710596780252,1.47584225705893));
#16627=CARTESIAN_POINT('Ctrl Pts',(91.4793707631218,-1.65354614096831,1.45739889781873));
#16628=CARTESIAN_POINT('Ctrl Pts',(91.4815174627805,-1.6791686944301,1.42766246014448));
#16629=CARTESIAN_POINT('Ctrl Pts',(91.4823084792419,-1.688554971239,1.4165485264697));
#16630=CARTESIAN_POINT('Ctrl Pts',(91.483776805428,-1.70587152075336,1.39562795113253));
#16631=CARTESIAN_POINT('Ctrl Pts',(91.4844552060113,-1.71382894303037,1.38584464732226));
#16632=CARTESIAN_POINT('Ctrl Pts',(91.4859774240675,-1.73158288037588,1.36363015860112));
#16633=CARTESIAN_POINT('Ctrl Pts',(91.486819261979,-1.74133039584258,1.35116059418951));
#16634=CARTESIAN_POINT('Ctrl Pts',(91.489328478301,-1.77015958708026,1.31345047701963));
#16635=CARTESIAN_POINT('Ctrl Pts',(91.4909799468487,-1.78883331948359,1.28790240581569));
#16636=CARTESIAN_POINT('Ctrl Pts',(91.4947491260432,-1.83066877875324,1.22799985983965));
#16637=CARTESIAN_POINT('Ctrl Pts',(91.4968523060118,-1.85342509817297,1.19337650818241));
#16638=CARTESIAN_POINT('Ctrl Pts',(91.5044172079401,-1.93272958052811,1.0649703041475));
#16639=CARTESIAN_POINT('Ctrl Pts',(91.5096995520165,-1.98324583884367,0.96764811528813));
#16640=CARTESIAN_POINT('Ctrl Pts',(91.5210940804545,-2.0759772333159,0.750912928935033));
#16641=CARTESIAN_POINT('Ctrl Pts',(91.527189841773,-2.11556595370753,0.63081340941809));
#16642=CARTESIAN_POINT('Ctrl Pts',(91.5348377651341,-2.14938557500779,0.488035531981092));
#16643=CARTESIAN_POINT('Ctrl Pts',(91.5359198798327,-2.15383579872805,0.468004618669745));
#16644=CARTESIAN_POINT('Ctrl Pts',(91.5375134493021,-2.15989300235521,0.438821687131036));
#16645=CARTESIAN_POINT('Ctrl Pts',(91.5380130469979,-2.16172292181633,0.429716485297551));
#16646=CARTESIAN_POINT('Ctrl Pts',(91.5389046743222,-2.16486547723034,0.413551718194397));
#16647=CARTESIAN_POINT('Ctrl Pts',(91.5392953981207,-2.16620123892506,0.406496923906515));
#16648=CARTESIAN_POINT('Ctrl Pts',(91.5401485414847,-2.16902809379142,0.391157239176011));
#16649=CARTESIAN_POINT('Ctrl Pts',(91.5406116421218,-2.17050618442878,0.382870416649713));
#16650=CARTESIAN_POINT('Ctrl Pts',(91.5419397911224,-2.17458671010755,0.359209914847188));
#16651=CARTESIAN_POINT('Ctrl Pts',(91.5428109411612,-2.17707346922702,0.343817108458859));
#16652=CARTESIAN_POINT('Ctrl Pts',(91.5448145660014,-2.18237051306425,0.308663725131759));
#16653=CARTESIAN_POINT('Ctrl Pts',(91.5459518012419,-2.18507608418323,0.288888917409796));
#16654=CARTESIAN_POINT('Ctrl Pts',(91.5557129420421,-2.20580301674085,0.120387726461102));
#16655=CARTESIAN_POINT('Ctrl Pts',(91.564849446274,-2.20888459567789,-0.0297765807555846));
#16656=CARTESIAN_POINT('Ctrl Pts',(91.5813600640831,-2.18641846177745,-0.305349903894416));
#16657=CARTESIAN_POINT('Ctrl Pts',(91.5887617838061,-2.16525710446567,-0.430504484890412));
#16658=CARTESIAN_POINT('Ctrl Pts',(91.5971927709482,-2.12728360785889,-0.576961809773478));
#16659=CARTESIAN_POINT('Ctrl Pts',(91.5985501440626,-2.1207149871722,-0.600656716048967));
#16660=CARTESIAN_POINT('Ctrl Pts',(91.6006886795398,-2.10963887385296,-0.63816190934446));
#16661=CARTESIAN_POINT('Ctrl Pts',(91.6014781359966,-2.1053891159868,-0.652045615807265));
#16662=CARTESIAN_POINT('Ctrl Pts',(91.602944953952,-2.09719202497965,-0.677909042259047));
#16663=CARTESIAN_POINT('Ctrl Pts',(91.6036233886024,-2.09327847008446,-0.689898771617686));
#16664=CARTESIAN_POINT('Ctrl Pts',(91.6051474582162,-2.08421110636715,-0.716890266186869));
#16665=CARTESIAN_POINT('Ctrl Pts',(91.6059910905471,-2.07899780249331,-0.731871399031573));
#16666=CARTESIAN_POINT('Ctrl Pts',(91.6085118097496,-2.06283882042617,-0.776739976308074));
#16667=CARTESIAN_POINT('Ctrl Pts',(91.610172758436,-2.05140680688962,-0.806448533546961));
#16668=CARTESIAN_POINT('Ctrl Pts',(91.613967368431,-2.02350234654679,-0.874526693965781));
#16669=CARTESIAN_POINT('Ctrl Pts',(91.61608620494,-2.00657500557723,-0.912696931455176));
#16670=CARTESIAN_POINT('Ctrl Pts',(91.623742500892,-1.94068508660386,-1.050567054278));
#16671=CARTESIAN_POINT('Ctrl Pts',(91.6290953902265,-1.88529029342755,-1.14700993441016));
#16672=CARTESIAN_POINT('Ctrl Pts',(91.6404537402205,-1.75321620865761,-1.34134277806872));
#16673=CARTESIAN_POINT('Ctrl Pts',(91.6464448151753,-1.67506129404871,-1.43775194858175));
#16674=CARTESIAN_POINT('Ctrl Pts',(91.653974394663,-1.57495580647477,-1.5419321637822));
#16675=CARTESIAN_POINT('Ctrl Pts',(91.6550609477213,-1.56047176233966,-1.55658870891824));
#16676=CARTESIAN_POINT('Ctrl Pts',(91.6566598595932,-1.53915392840911,-1.57756385653583));
#16677=CARTESIAN_POINT('Ctrl Pts',(91.657160247883,-1.53248185702167,-1.58404604995512));
#16678=CARTESIAN_POINT('Ctrl Pts',(91.6580527425156,-1.52058634066934,-1.59545753955939));
#16679=CARTESIAN_POINT('Ctrl Pts',(91.6584435332603,-1.5153795583386,-1.6004038155088));
#16680=CARTESIAN_POINT('Ctrl Pts',(91.6592961754356,-1.50402471161696,-1.61108545850678));
#16681=CARTESIAN_POINT('Ctrl Pts',(91.6597587006576,-1.49786806769339,-1.61681103866241));
#16682=CARTESIAN_POINT('Ctrl Pts',(91.6610834479012,-1.48023736115415,-1.63302018170824));
#16683=CARTESIAN_POINT('Ctrl Pts',(91.66195172347,-1.4686851810235,-1.64341758853522));
#16684=CARTESIAN_POINT('Ctrl Pts',(91.6697166066552,-1.36530253341888,-1.73450532860287));
#16685=CARTESIAN_POINT('Ctrl Pts',(91.6770487328687,-1.26702414325333,-1.80754095284121));
#16686=CARTESIAN_POINT('Ctrl Pts',(91.6942956777497,-1.02318000030342,-1.95905523859537));
#16687=CARTESIAN_POINT('Ctrl Pts',(91.7041330887592,-0.873807593510924,
-2.03009147201441));
#16688=CARTESIAN_POINT('Ctrl Pts',(91.71492361511,-0.691996546468892,-2.09272714715062));
#16689=CARTESIAN_POINT('Ctrl Pts',(91.7164450489779,-0.665936806524459,
-2.10116500961688));
#16690=CARTESIAN_POINT('Ctrl Pts',(91.7188538399707,-0.624002490387734,
-2.113884305136));
#16691=CARTESIAN_POINT('Ctrl Pts',(91.7197512553216,-0.608226152910891,
-2.11847750308101));
#16692=CARTESIAN_POINT('Ctrl Pts',(91.721338645453,-0.58005124675161,-2.12633979111678));
#16693=CARTESIAN_POINT('Ctrl Pts',(91.7220308361001,-0.567672868549915,
-2.12967788178312));
#16694=CARTESIAN_POINT('Ctrl Pts',(91.7234752066212,-0.541652686219961,
-2.13645178890026));
#16695=CARTESIAN_POINT('Ctrl Pts',(91.7242266415553,-0.528005664285126,
-2.13986539526126));
#16696=CARTESIAN_POINT('Ctrl Pts',(91.7262019539813,-0.49184833557254,-2.14854266681873));
#16697=CARTESIAN_POINT('Ctrl Pts',(91.7274186551605,-0.46928598861023,-2.15358331408037));
#16698=CARTESIAN_POINT('Ctrl Pts',(91.7336079355327,-0.353107999423411,
-2.17762604359026));
#16699=CARTESIAN_POINT('Ctrl Pts',(91.7383959974413,-0.258403858195734,
-2.19088350613045));
#16700=CARTESIAN_POINT('Ctrl Pts',(91.749536065119,-0.0320016969515925,
-2.20768685813454));
#16701=CARTESIAN_POINT('Ctrl Pts',(91.7557689060371,0.0997292633399901,
-2.20566491624735));
#16702=CARTESIAN_POINT('Ctrl Pts',(91.7636759866867,0.259382152033342,-2.18887661580208));
#16703=CARTESIAN_POINT('Ctrl Pts',(91.7651187476883,0.288209889429562,-2.18526769820067));
#16704=CARTESIAN_POINT('Ctrl Pts',(91.7689830054256,0.364256708917513,-2.17421653728006));
#16705=CARTESIAN_POINT('Ctrl Pts',(91.7714341207368,0.411317136494377,-2.16580657081204));
#16706=CARTESIAN_POINT('Ctrl Pts',(91.7746624002179,0.471029246601015,-2.15311939853649));
#16707=CARTESIAN_POINT('Ctrl Pts',(91.7753691712496,0.483969399437671,-2.15024772959854));
#16708=CARTESIAN_POINT('Ctrl Pts',(91.7765081951137,0.504592834162175,-2.14547540271095));
#16709=CARTESIAN_POINT('Ctrl Pts',(91.7769363102217,0.512293337088345,-2.14364972994317));
#16710=CARTESIAN_POINT('Ctrl Pts',(91.7777651821034,0.527099293794177,-2.1400551278568));
#16711=CARTESIAN_POINT('Ctrl Pts',(91.778165604664,0.534205988368107,-2.1382922092265));
#16712=CARTESIAN_POINT('Ctrl Pts',(91.7791419003741,0.551425687302881,-2.13392941414762));
#16713=CARTESIAN_POINT('Ctrl Pts',(91.7797198114331,0.561529200579008,-2.13129303033152));
#16714=CARTESIAN_POINT('Ctrl Pts',(91.7817996136798,0.597588802205233,-2.12160953119154));
#16715=CARTESIAN_POINT('Ctrl Pts',(91.783322248456,0.623433194688759,-2.11415947806979));
#16716=CARTESIAN_POINT('Ctrl Pts',(91.7872305614863,0.688578467176918,-2.09408199020002));
#16717=CARTESIAN_POINT('Ctrl Pts',(91.7896415002397,0.727672216614691,-2.08082014959478));
#16718=CARTESIAN_POINT('Ctrl Pts',(91.802606518549,0.933483177393505,-2.00449332548636));
#16719=CARTESIAN_POINT('Ctrl Pts',(91.8135193958348,1.09248855624563,-1.92246315836466));
#16720=CARTESIAN_POINT('Ctrl Pts',(91.8277320271604,1.2950213652082,-1.78465261417891));
#16721=CARTESIAN_POINT('Ctrl Pts',(91.8315240056046,1.34844031435482,-1.74464188907611));
#16722=CARTESIAN_POINT('Ctrl Pts',(91.8364127922964,1.41653783805181,-1.68863759162108));
#16723=CARTESIAN_POINT('Ctrl Pts',(91.8375927672744,1.43290998738678,-1.67476726040434));
#16724=CARTESIAN_POINT('Ctrl Pts',(91.8395107369848,1.45940843057469,-1.65164494633508));
#16725=CARTESIAN_POINT('Ctrl Pts',(91.8402544735503,1.46965526582547,-1.64253383756608));
#16726=CARTESIAN_POINT('Ctrl Pts',(91.8416927119705,1.48941131819245,-1.62463459027004));
#16727=CARTESIAN_POINT('Ctrl Pts',(91.8423876183539,1.49892941153607,-1.61585712728249));
#16728=CARTESIAN_POINT('Ctrl Pts',(91.8440169256429,1.52117671096957,-1.59497521473353));
#16729=CARTESIAN_POINT('Ctrl Pts',(91.8449482945539,1.53383975000811,-1.58280136685571));
#16730=CARTESIAN_POINT('Ctrl Pts',(91.8480555567873,1.5758834056257,-1.54140346188619));
#16731=CARTESIAN_POINT('Ctrl Pts',(91.8502016896559,1.60458593802326,-1.51150170165982));
#16732=CARTESIAN_POINT('Ctrl Pts',(91.8553554381694,1.67243024209419,-1.43671069857977));
#16733=CARTESIAN_POINT('Ctrl Pts',(91.8583273949453,1.71062931436566,-1.39100989155555));
#16734=CARTESIAN_POINT('Ctrl Pts',(91.8659189541454,1.80467201948883,-1.26875636994954));
#16735=CARTESIAN_POINT('Ctrl Pts',(91.8704642064856,1.857514646127,-1.19005191723368));
#16736=CARTESIAN_POINT('Ctrl Pts',(91.8765366517972,1.92054919879009,-1.08168713051415));
#16737=CARTESIAN_POINT('Ctrl Pts',(91.8780261522123,1.93541228142226,-1.05486280081008));
#16738=CARTESIAN_POINT('Ctrl Pts',(91.883733348176,1.98980363117531,-0.951677504658571));
#16739=CARTESIAN_POINT('Ctrl Pts',(91.8880186790286,2.02540778144843,-0.873343588386556));
#16740=CARTESIAN_POINT('Ctrl Pts',(91.8933376123173,2.06176373595543,-0.779084854719754));
#16741=CARTESIAN_POINT('Ctrl Pts',(91.894137974545,2.06704022049623,-0.764975565514932));
#16742=CARTESIAN_POINT('Ctrl Pts',(91.8953972268463,2.07503180512173,-0.742919582378854));
#16743=CARTESIAN_POINT('Ctrl Pts',(91.8958504619992,2.07784690980209,-0.735009328402896));
#16744=CARTESIAN_POINT('Ctrl Pts',(91.8966927851086,2.08296410203773,-0.720366005703706));
#16745=CARTESIAN_POINT('Ctrl Pts',(91.8970811282799,2.08527886270637,-0.713637648015302));
#16746=CARTESIAN_POINT('Ctrl Pts',(91.8979890650241,2.09058822154249,-0.697958431430296));
#16747=CARTESIAN_POINT('Ctrl Pts',(91.8985100702102,2.09355793715396,-0.688999449306322));
#16748=CARTESIAN_POINT('Ctrl Pts',(91.9001893186055,2.10288820661926,-0.660234741274431));
#16749=CARTESIAN_POINT('Ctrl Pts',(91.9013594253114,2.10902576190551,-0.640358489123532));
#16750=CARTESIAN_POINT('Ctrl Pts',(91.9079172659481,2.14149294730569,-0.529680978739443));
#16751=CARTESIAN_POINT('Ctrl Pts',(91.9135409171221,2.16223834853384,-0.437351568571615));
#16752=CARTESIAN_POINT('Ctrl Pts',(91.9296044761519,2.20404566552599,-0.17276353793493));
#16753=CARTESIAN_POINT('Ctrl Pts',(91.9400431913294,2.21080998527135,0.00108088287678498));
#16754=CARTESIAN_POINT('Ctrl Pts',(91.9519407566671,2.19420681588039,0.210809556561447));
#16755=CARTESIAN_POINT('Ctrl Pts',(91.9540050115326,2.19035975198268,0.247605755228386));
#16756=CARTESIAN_POINT('Ctrl Pts',(91.956970004875,2.18340907772031,0.301041848292649));
#16757=CARTESIAN_POINT('Ctrl Pts',(91.9578934654244,2.1810374218173,0.317769070498981));
#16758=CARTESIAN_POINT('Ctrl Pts',(91.9595106911321,2.17651784310179,0.34720624128054));
#16759=CARTESIAN_POINT('Ctrl Pts',(91.9602069624109,2.17445033473915,0.359927557905491));
#16760=CARTESIAN_POINT('Ctrl Pts',(91.961644278822,2.16992933580395,0.386283007250181));
#16761=CARTESIAN_POINT('Ctrl Pts',(91.9623847440086,2.1674586451363,0.399913637824268));
#16762=CARTESIAN_POINT('Ctrl Pts',(91.9642970407964,2.16070976558687,0.435245342066936));
#16763=CARTESIAN_POINT('Ctrl Pts',(91.9654625242916,2.15623307281403,0.456907191456433));
#16764=CARTESIAN_POINT('Ctrl Pts',(91.970854196108,2.13382902221312,0.557640559977619));
#16765=CARTESIAN_POINT('Ctrl Pts',(91.974950808638,2.11187274300309,0.635755125075461));
#16766=CARTESIAN_POINT('Ctrl Pts',(91.9891047253716,2.01936727305806,0.906545543536755));
#16767=CARTESIAN_POINT('Ctrl Pts',(91.99854707361,1.92632764621014,1.09037139324226));
#16768=CARTESIAN_POINT('Ctrl Pts',(92.0104608247405,1.79462730077302,1.27968124931439));
#16769=CARTESIAN_POINT('Ctrl Pts',(92.0118015169946,1.77964444597949,1.30043715122988));
#16770=CARTESIAN_POINT('Ctrl Pts',(92.0137257325496,1.75799438274974,1.32935420012301));
#16771=CARTESIAN_POINT('Ctrl Pts',(92.0142903517085,1.75162443324855,1.33773639968258));
#16772=CARTESIAN_POINT('Ctrl Pts',(92.0152515795808,1.74075785871653,1.35182500920623));
#16773=CARTESIAN_POINT('Ctrl Pts',(92.015646025913,1.73629253518679,1.35755552725237));
#16774=CARTESIAN_POINT('Ctrl Pts',(92.0164714375588,1.72693819155161,1.36943865788802));
#16775=CARTESIAN_POINT('Ctrl Pts',(92.0169027144122,1.72204451074607,1.37558731245748));
#16776=CARTESIAN_POINT('Ctrl Pts',(92.0180535727462,1.70896633641264,1.39184020007513));
#16777=CARTESIAN_POINT('Ctrl Pts',(92.0187770201623,1.70072524786362,1.40189824739245));
#16778=CARTESIAN_POINT('Ctrl Pts',(92.0223214531359,1.66022444146323,1.45044576832971));
#16779=CARTESIAN_POINT('Ctrl Pts',(92.0252177974617,1.62674658586073,1.4878954729299));
#16780=CARTESIAN_POINT('Ctrl Pts',(92.0346999724233,1.51490764521916,1.60471344520302));
#16781=CARTESIAN_POINT('Ctrl Pts',(92.0414524162853,1.43179417154656,1.67928997591744));
#16782=CARTESIAN_POINT('Ctrl Pts',(92.0557939701127,1.24195948820453,1.82524650235054));
#16783=CARTESIAN_POINT('Ctrl Pts',(92.063325517908,1.13391187701719,1.89426502704868));
#16784=CARTESIAN_POINT('Ctrl Pts',(92.072270166758,0.992819653283209,1.96796810016855));
#16785=CARTESIAN_POINT('Ctrl Pts',(92.0740032226068,0.964862797213367,1.98182472242866));
#16786=CARTESIAN_POINT('Ctrl Pts',(92.0765909358015,0.922186271688614,2.00185981846796));
#16787=CARTESIAN_POINT('Ctrl Pts',(92.0774607104127,0.90767905635058,2.00847927596927));
#16788=CARTESIAN_POINT('Ctrl Pts',(92.0790154608451,0.881457341838468,2.02010177086763));
#16789=CARTESIAN_POINT('Ctrl Pts',(92.0797023651437,0.869768995323809,2.02516175018502));
#16790=CARTESIAN_POINT('Ctrl Pts',(92.081164233774,0.844676062666869,2.03576736427398));
#16791=CARTESIAN_POINT('Ctrl Pts',(92.0819381399571,0.831259220410901,2.04128257096149));
#16792=CARTESIAN_POINT('Ctrl Pts',(92.0840427234432,0.794418110215777,2.05600322277211));
#16793=CARTESIAN_POINT('Ctrl Pts',(92.0853643974157,0.770888713594534,2.06494068814135));
#16794=CARTESIAN_POINT('Ctrl Pts',(92.0945362357198,0.605001546982336,2.12472089565496));
#16795=CARTESIAN_POINT('Ctrl Pts',(92.1018839744866,0.457895477860774,2.16120416521849));
#16796=CARTESIAN_POINT('Ctrl Pts',(92.1141757669867,0.206092714154166,2.19676480157138));
#16797=CARTESIAN_POINT('Ctrl Pts',(92.1191372854593,0.103106355978515,2.20399999999999));
#16798=CARTESIAN_POINT('Ctrl Pts',(92.1243308360554,1.24855421140824E-11,
2.20399999999999));
#16799=CARTESIAN_POINT('Origin',(66.9212607628943,0.,0.));
#16800=CARTESIAN_POINT('',(92.9850149380438,-5.17304578464428E-12,2.204));
#16801=CARTESIAN_POINT('',(92.8757411398941,1.22339489286472E-10,2.204));
#16802=CARTESIAN_POINT('',(66.9212607628943,-2.69912154532077E-16,2.204));
#16803=CARTESIAN_POINT('',(92.2357264933075,-0.00128844900583903,2.20399983654467));
#16804=CARTESIAN_POINT('Ctrl Pts',(92.9850149380438,-5.17304578464428E-12,
2.204));
#16805=CARTESIAN_POINT('Ctrl Pts',(92.9849839122787,0.000639203858989945,
2.204));
#16806=CARTESIAN_POINT('Ctrl Pts',(92.9849528833965,0.00127841658233731,
2.20399972192954));
#16807=CARTESIAN_POINT('Ctrl Pts',(92.9797323214733,0.108815440439529,2.20390615691735));
#16808=CARTESIAN_POINT('Ctrl Pts',(92.974478251419,0.215553806951163,2.19603613966628));
#16809=CARTESIAN_POINT('Ctrl Pts',(92.9680527442138,0.336335811111836,2.17823910869595));
#16810=CARTESIAN_POINT('Ctrl Pts',(92.9672447349579,0.351361136673496,2.17586596982931));
#16811=CARTESIAN_POINT('Ctrl Pts',(92.9659786535206,0.374623324503134,2.17194465465864));
#16812=CARTESIAN_POINT('Ctrl Pts',(92.9655264029516,0.382878224169359,2.17050465996205));
#16813=CARTESIAN_POINT('Ctrl Pts',(92.9646859458543,0.398112959507861,2.16775748114263));
#16814=CARTESIAN_POINT('Ctrl Pts',(92.9642984812101,0.405094919564516,2.16646359935022));
#16815=CARTESIAN_POINT('Ctrl Pts',(92.9634006733272,0.421178842820127,2.16340249362275));
#16816=CARTESIAN_POINT('Ctrl Pts',(92.9628890277217,0.430275993989048,2.16161155846629));
#16817=CARTESIAN_POINT('Ctrl Pts',(92.9612537321165,0.4591452608254,2.15573867343655));
#16818=CARTESIAN_POINT('Ctrl Pts',(92.960118947242,0.478872181017981,2.15144253327758));
#16819=CARTESIAN_POINT('Ctrl Pts',(92.9539006013826,0.585509899658901,2.12667966949229));
#16820=CARTESIAN_POINT('Ctrl Pts',(92.9486045419589,0.671168781968484,2.10121824082946));
#16821=CARTESIAN_POINT('Ctrl Pts',(92.933819310583,0.903071985138849,2.01665670528945));
#16822=CARTESIAN_POINT('Ctrl Pts',(92.9242974386048,1.04490898995667,1.94695132625936));
#16823=CARTESIAN_POINT('Ctrl Pts',(92.9122357445336,1.22253376590112,1.8346091148031));
#16824=CARTESIAN_POINT('Ctrl Pts',(92.9092709747304,1.26594452711196,1.80492784435747));
#16825=CARTESIAN_POINT('Ctrl Pts',(92.9052768022982,1.32407975285801,1.76204865563998));
#16826=CARTESIAN_POINT('Ctrl Pts',(92.904197761914,1.33974792228667,1.75016519132171));
#16827=CARTESIAN_POINT('Ctrl Pts',(92.9024777542054,1.36465654354071,1.73074279950544));
#16828=CARTESIAN_POINT('Ctrl Pts',(92.90183161925,1.37399825171393,1.72333598929291));
#16829=CARTESIAN_POINT('Ctrl Pts',(92.9004964246188,1.393267479012,1.70780160623859));
#16830=CARTESIAN_POINT('Ctrl Pts',(92.8998078689158,1.40318506811633,1.69966239841522));
#16831=CARTESIAN_POINT('Ctrl Pts',(92.8981903778024,1.4264317070319,1.68024209092026));
#16832=CARTESIAN_POINT('Ctrl Pts',(92.8972644608044,1.43969897980819,1.66888818381006));
#16833=CARTESIAN_POINT('Ctrl Pts',(92.8941624146894,1.48399128840569,1.63006226772277));
#16834=CARTESIAN_POINT('Ctrl Pts',(92.8920161254101,1.51437700350201,1.60187256617595));
#16835=CARTESIAN_POINT('Ctrl Pts',(92.8868545313899,1.58654273916021,1.53103239358963));
#16836=CARTESIAN_POINT('Ctrl Pts',(92.8838752364433,1.62742016329827,1.48750875411669));
#16837=CARTESIAN_POINT('Ctrl Pts',(92.8762792536898,1.72842160532998,1.37081453465306));
#16838=CARTESIAN_POINT('Ctrl Pts',(92.8717365304916,1.785687956913,1.29533495886259));
#16839=CARTESIAN_POINT('Ctrl Pts',(92.8656308010742,1.85525689813687,1.19022016947047));
#16840=CARTESIAN_POINT('Ctrl Pts',(92.86410524841,1.87202714204781,1.16366513212299));
#16841=CARTESIAN_POINT('Ctrl Pts',(92.8583877438188,1.93227596821877,1.06358845770907));
#16842=CARTESIAN_POINT('Ctrl Pts',(92.8541286082913,1.97203320318755,0.98792360780754));
#16843=CARTESIAN_POINT('Ctrl Pts',(92.8488443193015,2.01347217265633,0.896531896249151));
#16844=CARTESIAN_POINT('Ctrl Pts',(92.8480496416932,2.01950867408486,0.882850113037087));
#16845=CARTESIAN_POINT('Ctrl Pts',(92.8468001193165,2.02868709726872,0.861460343411248));
#16846=CARTESIAN_POINT('Ctrl Pts',(92.8463508577373,2.0319254780675,0.853793949886412));
#16847=CARTESIAN_POINT('Ctrl Pts',(92.845516610347,2.0378233577995,0.839607967547692));
#16848=CARTESIAN_POINT('Ctrl Pts',(92.8451323630115,2.04049512523086,0.833093761964362));
#16849=CARTESIAN_POINT('Ctrl Pts',(92.8442353798318,2.04662909675851,0.817931606398258));
#16850=CARTESIAN_POINT('Ctrl Pts',(92.8437212781954,2.0500677244246,0.80927442272493));
#16851=CARTESIAN_POINT('Ctrl Pts',(92.8420701584996,2.06087114413694,0.781564691370285));
#16852=CARTESIAN_POINT('Ctrl Pts',(92.840921711227,2.06802578976791,0.762431971692556));
#16853=CARTESIAN_POINT('Ctrl Pts',(92.8345558829956,2.10580332263445,0.656962710964858));
#16854=CARTESIAN_POINT('Ctrl Pts',(92.8291155984555,2.13128426196491,0.568886872142082));
#16855=CARTESIAN_POINT('Ctrl Pts',(92.8137824224623,2.18694565302358,0.319164456967255));
#16856=CARTESIAN_POINT('Ctrl Pts',(92.8038694073796,2.20465093358873,0.155322261893016));
#16857=CARTESIAN_POINT('Ctrl Pts',(92.7918959682104,2.20379594361052,-0.0545865236937455));
#16858=CARTESIAN_POINT('Ctrl Pts',(92.789334834381,2.20219444976358,-0.100181273902928));
#16859=CARTESIAN_POINT('Ctrl Pts',(92.7857903024108,2.19794896114756,-0.164263953771485));
#16860=CARTESIAN_POINT('Ctrl Pts',(92.7847706303255,2.19648369726788,-0.182815972943825));
#16861=CARTESIAN_POINT('Ctrl Pts',(92.7830562586421,2.1936045862794,-0.214199634368179));
#16862=CARTESIAN_POINT('Ctrl Pts',(92.7823577716966,2.19231267284516,-0.227041226913029));
#16863=CARTESIAN_POINT('Ctrl Pts',(92.7809522101568,2.18947170944573,-0.252989721766818));
#16864=CARTESIAN_POINT('Ctrl Pts',(92.7802453260336,2.18791758036183,-0.266095542551742));
#16865=CARTESIAN_POINT('Ctrl Pts',(92.7785068998949,2.18378482410443,-0.29845817780594));
#16866=CARTESIAN_POINT('Ctrl Pts',(92.7774797131055,2.18106909012312,-0.317696550519678));
#16867=CARTESIAN_POINT('Ctrl Pts',(92.7735562992069,2.1696402348826,-0.391586157752993));
#16868=CARTESIAN_POINT('Ctrl Pts',(92.7707167938676,2.15912407540004,-0.445939836186519));
#16869=CARTESIAN_POINT('Ctrl Pts',(92.7633257056357,2.12586248930158,-0.588781454512491));
#16870=CARTESIAN_POINT('Ctrl Pts',(92.7588713118499,2.09964441200728,-0.676350266198253));
#16871=CARTESIAN_POINT('Ctrl Pts',(92.7475505550456,2.0187950360889,-0.895763048813044));
#16872=CARTESIAN_POINT('Ctrl Pts',(92.7407675123292,1.95667374291665,-1.02437526572849));
#16873=CARTESIAN_POINT('Ctrl Pts',(92.7320167468765,1.868370468802,-1.16942503150712));
#16874=CARTESIAN_POINT('Ctrl Pts',(92.7305878127241,1.85372467846659,-1.19250484156476));
#16875=CARTESIAN_POINT('Ctrl Pts',(92.728560972024,1.83272739442273,-1.22427195733206));
#16876=CARTESIAN_POINT('Ctrl Pts',(92.7279849069519,1.82673524765478,-1.23319497778753));
#16877=CARTESIAN_POINT('Ctrl Pts',(92.7270129250864,1.8165909122042,-1.24806492590057));
#16878=CARTESIAN_POINT('Ctrl Pts',(92.7266193482799,1.81247411146441,-1.25403596259071));
#16879=CARTESIAN_POINT('Ctrl Pts',(92.7258055638006,1.80394563154433,-1.26627600479977));
#16880=CARTESIAN_POINT('Ctrl Pts',(92.7253851438225,1.79953061608079,-1.27254246294123));
#16881=CARTESIAN_POINT('Ctrl Pts',(92.724281735946,1.78791692147766,-1.28884507500649));
#16882=CARTESIAN_POINT('Ctrl Pts',(92.7235953543537,1.78066650987759,-1.2988438364977));
#16883=CARTESIAN_POINT('Ctrl Pts',(92.7204644421927,1.74745581902342,-1.34384266082031));
#16884=CARTESIAN_POINT('Ctrl Pts',(92.7179632571069,1.72054650049254,-1.37812705347092));
#16885=CARTESIAN_POINT('Ctrl Pts',(92.7103854021319,1.63732690310113,-1.47791592766632));
#16886=CARTESIAN_POINT('Ctrl Pts',(92.7052007251412,1.57816478303736,-1.54093136455266));
#16887=CARTESIAN_POINT('Ctrl Pts',(92.690229040135,1.39722180558688,-1.71228071231178));
#16888=CARTESIAN_POINT('Ctrl Pts',(92.6805196466665,1.26691824372134,-1.81081969578041));
#16889=CARTESIAN_POINT('Ctrl Pts',(92.6698386065759,1.10334374869042,-1.9081409224567));
#16890=CARTESIAN_POINT('Ctrl Pts',(92.6683140058262,1.0794972000625,-1.92173231708979));
#16891=CARTESIAN_POINT('Ctrl Pts',(92.6659058619808,1.0410380108242,-1.94271036965767));
#16892=CARTESIAN_POINT('Ctrl Pts',(92.6650121476636,1.02658672266771,-1.95038545974326));
#16893=CARTESIAN_POINT('Ctrl Pts',(92.6634346381087,1.00076506810022,-1.96373284443257));
#16894=CARTESIAN_POINT('Ctrl Pts',(92.6627486111315,0.98942872237785,-1.96946901945875));
#16895=CARTESIAN_POINT('Ctrl Pts',(92.6613205586691,0.965609596319418,-1.98126389235353));
#16896=CARTESIAN_POINT('Ctrl Pts',(92.6605792255044,0.953117900533176,-1.98730339490451));
#16897=CARTESIAN_POINT('Ctrl Pts',(92.6586387337385,0.920092964202268,-2.0028873172942));
#16898=CARTESIAN_POINT('Ctrl Pts',(92.6574464053749,0.899467963614082,-2.01223410698139));
#16899=CARTESIAN_POINT('Ctrl Pts',(92.651553422794,0.79594274369162,-2.05723957426045));
#16900=CARTESIAN_POINT('Ctrl Pts',(92.647016204674,0.711047714751651,-2.08810272223797));
#16901=CARTESIAN_POINT('Ctrl Pts',(92.637963299853,0.534615917547711,-2.14023005865897));
#16902=CARTESIAN_POINT('Ctrl Pts',(92.6334642792863,0.443135930912989,-2.16102517955939));
#16903=CARTESIAN_POINT('Ctrl Pts',(92.6275891962034,0.323378896705407,-2.1803217392013));
#16904=CARTESIAN_POINT('Ctrl Pts',(92.6262499391514,0.296067885881175,-2.18419792439964));
#16905=CARTESIAN_POINT('Ctrl Pts',(92.6205270009926,0.179788234100803,-2.19848021273297));
#16906=CARTESIAN_POINT('Ctrl Pts',(92.6160731731659,0.0903101869764456,
-2.20396913466076));
#16907=CARTESIAN_POINT('Ctrl Pts',(92.6105656608284,-0.0142990247707454,
-2.20400503734064));
#16908=CARTESIAN_POINT('Ctrl Pts',(92.609765741015,-0.0293537274748027,
-2.2038559391864));
#16909=CARTESIAN_POINT('Ctrl Pts',(92.6085097060718,-0.0527485348309028,
-2.20338449432119));
#16910=CARTESIAN_POINT('Ctrl Pts',(92.6080592673582,-0.0610906027192511,
-2.20316898383981));
#16911=CARTESIAN_POINT('Ctrl Pts',(92.6072203564332,-0.0765331441649997,
-2.20268226644223));
#16912=CARTESIAN_POINT('Ctrl Pts',(92.6068326016046,-0.0836337601653857,
-2.20242409146915));
#16913=CARTESIAN_POINT('Ctrl Pts',(92.6059316997565,-0.100046966832361,
-2.20174782888358));
#16914=CARTESIAN_POINT('Ctrl Pts',(92.60541721759,-0.109358250564828,-2.20130499116922));
#16915=CARTESIAN_POINT('Ctrl Pts',(92.6037636372896,-0.13909996275363,-2.19970133201543));
#16916=CARTESIAN_POINT('Ctrl Pts',(92.6026130638315,-0.159516586107941,
-2.19831507005317));
#16917=CARTESIAN_POINT('Ctrl Pts',(92.5962240395545,-0.271574097740623,
-2.18913730628015));
#16918=CARTESIAN_POINT('Ctrl Pts',(92.5907610287505,-0.362671080610185,
-2.17590016885438));
#16919=CARTESIAN_POINT('Ctrl Pts',(92.5753404797683,-0.614474109666137,
-2.12305730906649));
#16920=CARTESIAN_POINT('Ctrl Pts',(92.5653650708357,-0.771971921337889,
-2.07099590966598));
#16921=CARTESIAN_POINT('Ctrl Pts',(92.5534020200614,-0.962649651465769,
-1.98315595359836));
#16922=CARTESIAN_POINT('Ctrl Pts',(92.550901449755,-1.00255169015041,-1.96328612289777));
#16923=CARTESIAN_POINT('Ctrl Pts',(92.5474262739442,-1.05805817806878,-1.93351188016115));
#16924=CARTESIAN_POINT('Ctrl Pts',(92.5464172104109,-1.07418093427552,-1.92460142586598));
#16925=CARTESIAN_POINT('Ctrl Pts',(92.5447153555933,-1.10137638250148,-1.9091232858247));
#16926=CARTESIAN_POINT('Ctrl Pts',(92.5440189054631,-1.11250649825665,-1.90265891782784));
#16927=CARTESIAN_POINT('Ctrl Pts',(92.5426131217319,-1.13497079642317,-1.88934714054745));
#16928=CARTESIAN_POINT('Ctrl Pts',(92.5419040227218,-1.14630117937367,-1.88249434074438));
#16929=CARTESIAN_POINT('Ctrl Pts',(92.5401520797203,-1.17428619620329,-1.86522219484113));
#16930=CARTESIAN_POINT('Ctrl Pts',(92.5391137458381,-1.19086475364906,-1.85468139541838));
#16931=CARTESIAN_POINT('Ctrl Pts',(92.5350873372309,-1.25508385264487,-1.81263415497283));
#16932=CARTESIAN_POINT('Ctrl Pts',(92.53216003712,-1.30163517357271,-1.77950123145934));
#16933=CARTESIAN_POINT('Ctrl Pts',(92.5244525251043,-1.42287635247538,-1.68590151859254));
#16934=CARTESIAN_POINT('Ctrl Pts',(92.519781355041,-1.49498825884334,-1.6222985684472));
#16935=CARTESIAN_POINT('Ctrl Pts',(92.5079801141876,-1.6670423277798,-1.44930005805614));
#16936=CARTESIAN_POINT('Ctrl Pts',(92.5009237560612,-1.76052346655767,-1.33418420393547));
#16937=CARTESIAN_POINT('Ctrl Pts',(92.492196633563,-1.85226066807786,-1.19461787178206));
#16938=CARTESIAN_POINT('Ctrl Pts',(92.4911865964675,-1.86255219363709,-1.17850783590741));
#16939=CARTESIAN_POINT('Ctrl Pts',(92.4896780473303,-1.87741656921542,-1.15455849845753));
#16940=CARTESIAN_POINT('Ctrl Pts',(92.4891896147057,-1.88215290009038,-1.14682115237109));
#16941=CARTESIAN_POINT('Ctrl Pts',(92.4883140808716,-1.89050377867012,-1.13298794576134));
#16942=CARTESIAN_POINT('Ctrl Pts',(92.4879281877325,-1.89413687342042,-1.12690360061047));
#16943=CARTESIAN_POINT('Ctrl Pts',(92.4870734863541,-1.90207869110663,-1.1134565205666));
#16944=CARTESIAN_POINT('Ctrl Pts',(92.4866038715698,-1.90637398503866,-1.10608634134698));
#16945=CARTESIAN_POINT('Ctrl Pts',(92.4852251319747,-1.91879012427482,-1.08449465576655));
#16946=CARTESIAN_POINT('Ctrl Pts',(92.4843091163201,-1.92679520605582,-1.07020764380351));
#16947=CARTESIAN_POINT('Ctrl Pts',(92.4771869694501,-1.98724411408087,-0.959444995656458));
#16948=CARTESIAN_POINT('Ctrl Pts',(92.470633533886,-2.03256660451294,-0.859268598926655));
#16949=CARTESIAN_POINT('Ctrl Pts',(92.4533310409448,-2.1314452370969,-0.588550426358175));
#16950=CARTESIAN_POINT('Ctrl Pts',(92.4426379332962,-2.1720914820329,-0.41411318277556));
#16951=CARTESIAN_POINT('Ctrl Pts',(92.4311841865796,-2.19404988115412,-0.210802711160837));
#16952=CARTESIAN_POINT('Ctrl Pts',(92.4297411883603,-2.19638512628893,-0.184892192079739));
#16953=CARTESIAN_POINT('Ctrl Pts',(92.4274268192586,-2.19942416530005,-0.142861447894437));
#16954=CARTESIAN_POINT('Ctrl Pts',(92.4265467168451,-2.2004105921066,-0.126764734242479));
#16955=CARTESIAN_POINT('Ctrl Pts',(92.4249865997517,-2.20185496766462,-0.0980331544618974));
#16956=CARTESIAN_POINT('Ctrl Pts',(92.4243044815661,-2.20238103161062,-0.0854025696111373));
#16957=CARTESIAN_POINT('Ctrl Pts',(92.4228663666374,-2.20326537717916,-0.0586320688867149));
#16958=CARTESIAN_POINT('Ctrl Pts',(92.4221112573544,-2.20359627333529,-0.0444917821840294));
#16959=CARTESIAN_POINT('Ctrl Pts',(92.4200917293518,-2.20412006431658,-0.00645680217045421));
#16960=CARTESIAN_POINT('Ctrl Pts',(92.4188352133837,-2.20406053916097,0.0174398040700708));
#16961=CARTESIAN_POINT('Ctrl Pts',(92.4116469659395,-2.20147357934064,0.155365518987877));
#16962=CARTESIAN_POINT('Ctrl Pts',(92.4059864301294,-2.1904865573394,0.269066775171342));
#16963=CARTESIAN_POINT('Ctrl Pts',(92.3963620201088,-2.1562810457452,0.46373941959347));
#16964=CARTESIAN_POINT('Ctrl Pts',(92.3923533820206,-2.13714530301353,0.545171569715213));
#16965=CARTESIAN_POINT('Ctrl Pts',(92.3833756488157,-2.08477275793679,0.722178251423084));
#16966=CARTESIAN_POINT('Ctrl Pts',(92.3783911481762,-2.0494925529869,0.816942369086879));
#16967=CARTESIAN_POINT('Ctrl Pts',(92.3722790322138,-2.00160837423168,0.922718036375735));
#16968=CARTESIAN_POINT('Ctrl Pts',(92.3714756925602,-1.99523076279892,0.936428767494364));
#16969=CARTESIAN_POINT('Ctrl Pts',(92.3702154099764,-1.9851091998815,0.95761544869857));
#16970=CARTESIAN_POINT('Ctrl Pts',(92.3697642046487,-1.98146282015777,0.965137798815417));
#16971=CARTESIAN_POINT('Ctrl Pts',(92.3689246429268,-1.97463892634774,0.979013570835433));
#16972=CARTESIAN_POINT('Ctrl Pts',(92.3685370143041,-1.97147339022142,0.985372583592353));
#16973=CARTESIAN_POINT('Ctrl Pts',(92.3676374366787,-1.96409230358272,1.0000219609404));
#16974=CARTESIAN_POINT('Ctrl Pts',(92.3671241665289,-1.95985497638065,1.00830102871188));
#16975=CARTESIAN_POINT('Ctrl Pts',(92.3654784150002,-1.94618130364127,1.03460537817979));
#16976=CARTESIAN_POINT('Ctrl Pts',(92.3643346046839,-1.93654796299813,1.05252642815279));
#16977=CARTESIAN_POINT('Ctrl Pts',(92.3580191343098,-1.88256706276936,1.14969753039784));
#16978=CARTESIAN_POINT('Ctrl Pts',(92.3526281480761,-1.8336048428453,1.22627636476325));
#16979=CARTESIAN_POINT('Ctrl Pts',(92.3374834448696,-1.68456818431785,1.43041052232648));
#16980=CARTESIAN_POINT('Ctrl Pts',(92.3277049785731,-1.57493166587011,1.55030547930311));
#16981=CARTESIAN_POINT('Ctrl Pts',(92.3157044236337,-1.41708671611664,1.6887214811619));
#16982=CARTESIAN_POINT('Ctrl Pts',(92.3130078931126,-1.38001264771135,1.71915112631692));
#16983=CARTESIAN_POINT('Ctrl Pts',(92.3093108689137,-1.32691074219027,1.75991034702617));
#16984=CARTESIAN_POINT('Ctrl Pts',(92.3082698497897,-1.31169912552376,1.77127693579941));
#16985=CARTESIAN_POINT('Ctrl Pts',(92.3065943744804,-1.28679956838745,1.78938595558961));
#16986=CARTESIAN_POINT('Ctrl Pts',(92.3059552414593,-1.2772012594229,1.79624947537518));
#16987=CARTESIAN_POINT('Ctrl Pts',(92.3046222458572,-1.25697483961603,1.81046880644041));
#16988=CARTESIAN_POINT('Ctrl Pts',(92.3039290011311,-1.24633618807167,1.81780889057594));
#16989=CARTESIAN_POINT('Ctrl Pts',(92.3022782017456,-1.22072012287885,1.83515196518747));
#16990=CARTESIAN_POINT('Ctrl Pts',(92.3013240267401,-1.20568333809347,1.84506587085693));
#16991=CARTESIAN_POINT('Ctrl Pts',(92.2980108198246,-1.1526844936187,1.87908393729929));
#16992=CARTESIAN_POINT('Ctrl Pts',(92.2956876417274,-1.11410661619497,1.90221050190376));
#16993=CARTESIAN_POINT('Ctrl Pts',(92.2899944942639,-1.01639330839061,1.95679421183827));
#16994=CARTESIAN_POINT('Ctrl Pts',(92.2866718568686,-0.956480355202978,
1.98676749736706));
#16995=CARTESIAN_POINT('Ctrl Pts',(92.277790410745,-0.79069248943156,2.06046713781154));
#16996=CARTESIAN_POINT('Ctrl Pts',(92.2723379247909,-0.682631086942057,
2.09874570079143));
#16997=CARTESIAN_POINT('Ctrl Pts',(92.2635807017027,-0.509891923156279,
2.14517457413493));
#16998=CARTESIAN_POINT('Ctrl Pts',(92.2603814935311,-0.446997420984935,
2.15915631174931));
#16999=CARTESIAN_POINT('Ctrl Pts',(92.2556018353007,-0.355505543634313,
2.17532639451038));
#17000=CARTESIAN_POINT('Ctrl Pts',(92.2541130197628,-0.32733317341784,2.17974355348617));
#17001=CARTESIAN_POINT('Ctrl Pts',(92.2520145308062,-0.288251538248025,
2.18509647440409));
#17002=CARTESIAN_POINT('Ctrl Pts',(92.2514287732939,-0.277408041027634,
2.18649955877926));
#17003=CARTESIAN_POINT('Ctrl Pts',(92.2504806093252,-0.259971924181495,
2.18862390005417));
#17004=CARTESIAN_POINT('Ctrl Pts',(92.2501210116239,-0.253385570763207,
2.1893962015553));
#17005=CARTESIAN_POINT('Ctrl Pts',(92.2493988040727,-0.240213485565602,
2.1908804987964));
#17006=CARTESIAN_POINT('Ctrl Pts',(92.2490361988305,-0.233627846944208,
2.1915925499295));
#17007=CARTESIAN_POINT('Ctrl Pts',(92.2482646760888,-0.219671376636344,
2.19303792794988));
#17008=CARTESIAN_POINT('Ctrl Pts',(92.2478553565435,-0.212299854477745,
2.19376380581684));
#17009=CARTESIAN_POINT('Ctrl Pts',(92.2468683636488,-0.194599233684011,
2.19541674582902));
#17010=CARTESIAN_POINT('Ctrl Pts',(92.2462888684194,-0.18426706517281,2.19630808176313));
#17011=CARTESIAN_POINT('Ctrl Pts',(92.2424670889475,-0.116489477121162,
2.20167349948885));
#17012=CARTESIAN_POINT('Ctrl Pts',(92.2391242511364,-0.058897880036256,
2.20396596668738));
#17013=CARTESIAN_POINT('Ctrl Pts',(92.2357268140388,-0.00128762525293467,
2.20399962387048));
#17014=CARTESIAN_POINT('Ctrl Pts',(92.2357268613305,-0.00128842717656291,
2.20399962340183));
#17015=CARTESIAN_POINT('Ctrl Pts',(92.2357015338201,-0.000858949161186015,
2.20399987446864));
#17016=CARTESIAN_POINT('Ctrl Pts',(92.2356762034427,-0.000429473425876918,
2.204));
#17017=CARTESIAN_POINT('Ctrl Pts',(92.2356508702176,-2.51612300885953E-11,
2.204));
#17018=CARTESIAN_POINT('',(92.1243948225064,-0.00126182935173377,2.20399987870527));
#17019=CARTESIAN_POINT('Ctrl Pts',(92.1243308360554,1.24847509279933E-11,
2.204));
#17020=CARTESIAN_POINT('Ctrl Pts',(92.1243520093957,-0.000420349403778188,
2.204));
#17021=CARTESIAN_POINT('Ctrl Pts',(92.1243731866753,-0.000840700810317714,
2.20399987974572));
#17022=CARTESIAN_POINT('Ctrl Pts',(92.1243943679136,-0.00126105415559237,
2.20399963923373));
#17023=CARTESIAN_POINT('Ctrl Pts',(92.1243944080205,-0.00126185009846303,
2.20399963877818));
#17024=CARTESIAN_POINT('Ctrl Pts',(92.1259360221631,-0.0318560252145767,
2.20398212277581));
#17025=CARTESIAN_POINT('Ctrl Pts',(92.1274978250993,-0.0624453826648012,
2.20332758254774));
#17026=CARTESIAN_POINT('Ctrl Pts',(92.1300489761317,-0.111503091054167,
2.20125547486973));
#17027=CARTESIAN_POINT('Ctrl Pts',(92.1310206936636,-0.129985052916093,
2.20024145237313));
#17028=CARTESIAN_POINT('Ctrl Pts',(92.1324632420578,-0.157072999238677,
2.19841277798702));
#17029=CARTESIAN_POINT('Ctrl Pts',(92.1329249119006,-0.165690890354302,
2.19778006031472));
#17030=CARTESIAN_POINT('Ctrl Pts',(92.1337572455189,-0.181129958988984,
2.19655521563871));
#17031=CARTESIAN_POINT('Ctrl Pts',(92.1341268966739,-0.187952566928249,
2.195981946057));
#17032=CARTESIAN_POINT('Ctrl Pts',(92.1348865159491,-0.201899683140805,
2.19474456768884));
#17033=CARTESIAN_POINT('Ctrl Pts',(92.1352766593163,-0.209023631101947,
2.19407755500457));
#17034=CARTESIAN_POINT('Ctrl Pts',(92.1361663608094,-0.225180764304435,
2.19248536478043));
#17035=CARTESIAN_POINT('Ctrl Pts',(92.1366670565733,-0.234211516058069,
2.19153905079146));
#17036=CARTESIAN_POINT('Ctrl Pts',(92.1382176937927,-0.261999662312857,
2.18845347062796));
#17037=CARTESIAN_POINT('Ctrl Pts',(92.1392771739789,-0.280735152572016,
2.18612903131721));
#17038=CARTESIAN_POINT('Ctrl Pts',(92.1438518035719,-0.360689571814189,
2.17516467516825));
#17039=CARTESIAN_POINT('Ctrl Pts',(92.1474675623071,-0.421556483211142,
2.16419207368789));
#17040=CARTESIAN_POINT('Ctrl Pts',(92.1588422795101,-0.608655046215802,
2.12227110613759));
#17041=CARTESIAN_POINT('Ctrl Pts',(92.1667394077557,-0.73267452599131,2.08271112846419));
#17042=CARTESIAN_POINT('Ctrl Pts',(92.1784325303129,-0.91494340669467,2.00626046433122));
#17043=CARTESIAN_POINT('Ctrl Pts',(92.1823797112768,-0.976158938583549,
1.97719938401971));
#17044=CARTESIAN_POINT('Ctrl Pts',(92.1880017006623,-1.06323302823782,1.93083077051992));
#17045=CARTESIAN_POINT('Ctrl Pts',(92.1897451893135,-1.09021510586326,1.91572521335551));
#17046=CARTESIAN_POINT('Ctrl Pts',(92.1928756481769,-1.13862301878099,1.88727057703892));
#17047=CARTESIAN_POINT('Ctrl Pts',(92.1942689731587,-1.16015407832838,1.87411184274326));
#17048=CARTESIAN_POINT('Ctrl Pts',(92.1964427904054,-1.1937119560621,1.852802896066));
#17049=CARTESIAN_POINT('Ctrl Pts',(92.1972322556332,-1.20589181141834,1.84489884792334));
#17050=CARTESIAN_POINT('Ctrl Pts',(92.1987057086537,-1.22860611343567,1.8298374747043));
#17051=CARTESIAN_POINT('Ctrl Pts',(92.1993907028663,-1.23915830324513,1.82270811562217));
#17052=CARTESIAN_POINT('Ctrl Pts',(92.2009245850578,-1.26276616081912,1.80645820106223));
#17053=CARTESIAN_POINT('Ctrl Pts',(92.2017714931534,-1.27578602985604,1.79728674205346));
#17054=CARTESIAN_POINT('Ctrl Pts',(92.2042567544561,-1.31393514562192,1.76979028153189));
#17055=CARTESIAN_POINT('Ctrl Pts',(92.2058799901889,-1.33877773858901,1.75107324232102));
#17056=CARTESIAN_POINT('Ctrl Pts',(92.2145873774472,-1.47138554872632,1.64669085357318));
#17057=CARTESIAN_POINT('Ctrl Pts',(92.2212827303238,-1.5713460582974,1.55159348236101));
#17058=CARTESIAN_POINT('Ctrl Pts',(92.2329681421634,-1.7301303783204,1.36933931830502));
#17059=CARTESIAN_POINT('Ctrl Pts',(92.2379688032933,-1.79283173979382,1.28615442069662));
#17060=CARTESIAN_POINT('Ctrl Pts',(92.2448386934838,-1.86713670133269,1.17152779623565));
#17061=CARTESIAN_POINT('Ctrl Pts',(92.2464989613227,-1.88424458565701,1.14380898826709));
#17062=CARTESIAN_POINT('Ctrl Pts',(92.2493660199057,-1.91218864747155,1.09620382574241));
#17063=CARTESIAN_POINT('Ctrl Pts',(92.2505564758016,-1.92334427413485,1.07651055534892));
#17064=CARTESIAN_POINT('Ctrl Pts',(92.2522860967265,-1.93887346540725,1.0480844171766));
#17065=CARTESIAN_POINT('Ctrl Pts',(92.2528105921555,-1.94349567256291,1.03948825095711));
#17066=CARTESIAN_POINT('Ctrl Pts',(92.2537291095489,-1.95143575171012,1.02448356806266));
#17067=CARTESIAN_POINT('Ctrl Pts',(92.254121508006,-1.95477948130486,1.01808902008186));
#17068=CARTESIAN_POINT('Ctrl Pts',(92.2549656211302,-1.96186814439548,1.00436898877901));
#17069=CARTESIAN_POINT('Ctrl Pts',(92.2554178774834,-1.96560342491157,0.997039042900629));
#17070=CARTESIAN_POINT('Ctrl Pts',(92.2566634879079,-1.97572350604232,0.976901948201957));
#17071=CARTESIAN_POINT('Ctrl Pts',(92.2574617242342,-1.9820246380984,0.964053473970097));
#17072=CARTESIAN_POINT('Ctrl Pts',(92.2619328683899,-2.01633511436113,0.89233349753733));
#17073=CARTESIAN_POINT('Ctrl Pts',(92.2657315141812,-2.04184463156987,0.832307306234299));
#17074=CARTESIAN_POINT('Ctrl Pts',(92.2776291130239,-2.11215097181134,0.64409423739175));
#17075=CARTESIAN_POINT('Ctrl Pts',(92.2858890129141,-2.14780109517018,0.51282732590043));
#17076=CARTESIAN_POINT('Ctrl Pts',(92.2998360268757,-2.18838459773861,0.280407187679906));
#17077=CARTESIAN_POINT('Ctrl Pts',(92.3056197596986,-2.19887030664066,0.180634844817134));
#17078=CARTESIAN_POINT('Ctrl Pts',(92.3124929664486,-2.20338392659665,0.0571149444333545));
#17079=CARTESIAN_POINT('Ctrl Pts',(92.3137818374172,-2.20386591726108,0.0337331161833779));
#17080=CARTESIAN_POINT('Ctrl Pts',(92.3158305365386,-2.20404202072537,-0.00377662077893416));
#17081=CARTESIAN_POINT('Ctrl Pts',(92.3165976868249,-2.20397256185814,-0.0179011626142755));
#17082=CARTESIAN_POINT('Ctrl Pts',(92.3180522176951,-2.20358127573999,-0.0448277041222772));
#17083=CARTESIAN_POINT('Ctrl Pts',(92.3187403257175,-2.20328364503262,-0.0576294280264321));
#17084=CARTESIAN_POINT('Ctrl Pts',(92.3202974585982,-2.20235301657398,-0.0867379788831724));
#17085=CARTESIAN_POINT('Ctrl Pts',(92.3211642726723,-2.20165044171183,-0.103041925719591));
#17086=CARTESIAN_POINT('Ctrl Pts',(92.323450364999,-2.19930521628583,-0.146291714071161));
#17087=CARTESIAN_POINT('Ctrl Pts',(92.3248598702747,-2.19734846081747,-0.173218140589351));
#17088=CARTESIAN_POINT('Ctrl Pts',(92.3366407252715,-2.17665637532275,-0.400186715694862));
#17089=CARTESIAN_POINT('Ctrl Pts',(92.346077812492,-2.13114630735586,-0.596823283658799));
#17090=CARTESIAN_POINT('Ctrl Pts',(92.3598546797665,-2.0308419927588,-0.860136345621305));
#17091=CARTESIAN_POINT('Ctrl Pts',(92.3638754506865,-1.99792506500616,-0.934048664990639));
#17092=CARTESIAN_POINT('Ctrl Pts',(92.3691090323471,-1.95218848187927,-1.02320624535878));
#17093=CARTESIAN_POINT('Ctrl Pts',(92.3701316843765,-1.94312466105778,-1.04031600504733));
#17094=CARTESIAN_POINT('Ctrl Pts',(92.3716584436675,-1.92943678936706,-1.06535149430467));
#17095=CARTESIAN_POINT('Ctrl Pts',(92.3721522105306,-1.92498654724541,-1.07337175173908));
#17096=CARTESIAN_POINT('Ctrl Pts',(92.3729999175782,-1.91731010568671,-1.08700500015952));
#17097=CARTESIAN_POINT('Ctrl Pts',(92.3733522627422,-1.91410904060029,-1.09263191026518));
#17098=CARTESIAN_POINT('Ctrl Pts',(92.3741613207157,-1.90673587928723,-1.10546078959782));
#17099=CARTESIAN_POINT('Ctrl Pts',(92.3746190344808,-1.90254783736073,-1.11265313219333));
#17100=CARTESIAN_POINT('Ctrl Pts',(92.3758940169671,-1.89083218626658,-1.13251348188617));
#17101=CARTESIAN_POINT('Ctrl Pts',(92.376716536809,-1.88321824754322,-1.14512975310402));
#17102=CARTESIAN_POINT('Ctrl Pts',(92.3816678300496,-1.83701300535474,-1.21998447349178));
#17103=CARTESIAN_POINT('Ctrl Pts',(92.3859548896681,-1.79546863117158,-1.28033957112359));
#17104=CARTESIAN_POINT('Ctrl Pts',(92.39789157381,-1.67352711280962,-1.43986017308734));
#17105=CARTESIAN_POINT('Ctrl Pts',(92.4056397829112,-1.58739416654353,-1.53429862117625));
#17106=CARTESIAN_POINT('Ctrl Pts',(92.4190658044793,-1.42032868681611,-1.68825467241441));
#17107=CARTESIAN_POINT('Ctrl Pts',(92.4248139314163,-1.34258318875831,-1.75071755643439));
#17108=CARTESIAN_POINT('Ctrl Pts',(92.4316521798041,-1.241715934637,-1.82107189948996));
#17109=CARTESIAN_POINT('Ctrl Pts',(92.4329392134088,-1.22235094164076,-1.83412637519782));
#17110=CARTESIAN_POINT('Ctrl Pts',(92.4349857090026,-1.19095189540914,-1.85457512064807));
#17111=CARTESIAN_POINT('Ctrl Pts',(92.4357524652561,-1.1790482674256,-1.86216553813707));
#17112=CARTESIAN_POINT('Ctrl Pts',(92.4372066884223,-1.15620864164595,-1.87642254933051));
#17113=CARTESIAN_POINT('Ctrl Pts',(92.437894877631,-1.14528589758854,-1.88310919201072));
#17114=CARTESIAN_POINT('Ctrl Pts',(92.4394527825923,-1.12030273312725,-1.89810550430086));
#17115=CARTESIAN_POINT('Ctrl Pts',(92.4403202793104,-1.10620690207326,-1.90635490623168));
#17116=CARTESIAN_POINT('Ctrl Pts',(92.4430440524502,-1.06137952753207,-1.93192490511823));
#17117=CARTESIAN_POINT('Ctrl Pts',(92.4448796432446,-1.03032244091916,-1.94866523271354));
#17118=CARTESIAN_POINT('Ctrl Pts',(92.4557216018491,-0.842192626441297,
-2.04431482303175));
#17119=CARTESIAN_POINT('Ctrl Pts',(92.4640675978479,-0.676548511763246,
-2.10494572099715));
#17120=CARTESIAN_POINT('Ctrl Pts',(92.4772388693823,-0.412688936544367,
-2.16711488874979));
#17121=CARTESIAN_POINT('Ctrl Pts',(92.481927782874,-0.318611853834009,-2.18292973534898));
#17122=CARTESIAN_POINT('Ctrl Pts',(92.4879789158816,-0.203047280456454,
-2.19472633107972));
#17123=CARTESIAN_POINT('Ctrl Pts',(92.4890794242496,-0.182249458261284,
-2.19655114642823));
#17124=CARTESIAN_POINT('Ctrl Pts',(92.4907005858738,-0.152002880936595,
-2.19877249090341));
#17125=CARTESIAN_POINT('Ctrl Pts',(92.4912089806292,-0.142571967361765,
-2.19940413977913));
#17126=CARTESIAN_POINT('Ctrl Pts',(92.4921060840201,-0.126033420959466,
-2.20040501475885));
#17127=CARTESIAN_POINT('Ctrl Pts',(92.4924933360493,-0.118927639343395,
-2.20080050604638));
#17128=CARTESIAN_POINT('Ctrl Pts',(92.4933412698498,-0.103443247750162,
-2.20158711917442));
#17129=CARTESIAN_POINT('Ctrl Pts',(92.4938026491174,-0.0950644096843052,
-2.20196482761502));
#17130=CARTESIAN_POINT('Ctrl Pts',(92.4950974853735,-0.0716717406611916,
-2.20288557840956));
#17131=CARTESIAN_POINT('Ctrl Pts',(92.4959364494406,-0.056654484276065,
-2.20332293458561));
#17132=CARTESIAN_POINT('Ctrl Pts',(92.5015412717844,0.0428487503805245,
-2.20520292228096));
#17133=CARTESIAN_POINT('Ctrl Pts',(92.5065177207575,0.127346452643196,-2.20193919230552));
#17134=CARTESIAN_POINT('Ctrl Pts',(92.5134635695193,0.243156214577335,-2.19077756755995));
#17135=CARTESIAN_POINT('Ctrl Pts',(92.5153749179594,0.274802606981332,-2.18703332863539));
#17136=CARTESIAN_POINT('Ctrl Pts',(92.5228252200121,0.397649971600758,-2.16979013569201));
#17137=CARTESIAN_POINT('Ctrl Pts',(92.5283692401964,0.488053878794831,-2.15126000416897));
#17138=CARTESIAN_POINT('Ctrl Pts',(92.5392243809405,0.665981258996695,-2.10299279767138));
#17139=CARTESIAN_POINT('Ctrl Pts',(92.5445247469296,0.753334519271191,-2.07330658230774));
#17140=CARTESIAN_POINT('Ctrl Pts',(92.5509200340969,0.859765848346851,-2.02951803232778));
#17141=CARTESIAN_POINT('Ctrl Pts',(92.5521819456515,0.880813883539689,-2.02047215176543));
#17142=CARTESIAN_POINT('Ctrl Pts',(92.554198290323,0.914512121573808,-2.00536285679522));
#17143=CARTESIAN_POINT('Ctrl Pts',(92.5549596411075,0.927251761732526,-1.99950413629387));
#17144=CARTESIAN_POINT('Ctrl Pts',(92.5564097235289,0.951541478150501,-1.98805167874642));
#17145=CARTESIAN_POINT('Ctrl Pts',(92.55709910629,0.963100271670365,-1.98247787840536));
#17146=CARTESIAN_POINT('Ctrl Pts',(92.5586680173806,0.989426766877393,-1.96949830576375));
#17147=CARTESIAN_POINT('Ctrl Pts',(92.559545209038,1.00416129508404,-1.96202676254249));
#17148=CARTESIAN_POINT('Ctrl Pts',(92.5618784290095,1.04337853530288,-1.94158307338858));
#17149=CARTESIAN_POINT('Ctrl Pts',(92.563324009837,1.06770335515914,-1.92831357229155));
#17150=CARTESIAN_POINT('Ctrl Pts',(92.5730185367437,1.2307808021807,-1.83532052139995));
#17151=CARTESIAN_POINT('Ctrl Pts',(92.5807141111319,1.3607433410048,-1.74115056363579));
#17152=CARTESIAN_POINT('Ctrl Pts',(92.5945655181774,1.57304189210383,-1.54891050962903));
#17153=CARTESIAN_POINT('Ctrl Pts',(92.6006958734549,1.65923325915252,-1.45620122665279));
#17154=CARTESIAN_POINT('Ctrl Pts',(92.6081644098687,1.74662289606223,-1.34430985196332));
#17155=CARTESIAN_POINT('Ctrl Pts',(92.6089948028617,1.7561163470124,-1.33188432954069));
#17156=CARTESIAN_POINT('Ctrl Pts',(92.6102863273112,1.77052140091805,-1.31260846873266));
#17157=CARTESIAN_POINT('Ctrl Pts',(92.6107411911895,1.77552744689428,-1.30582897189404));
#17158=CARTESIAN_POINT('Ctrl Pts',(92.6115885916867,1.78472598476277,-1.29322105823049));
#17159=CARTESIAN_POINT('Ctrl Pts',(92.6119803990189,1.78892902163402,-1.28740067461467));
#17160=CARTESIAN_POINT('Ctrl Pts',(92.6128828482631,1.79849649270917,-1.27401428005548));
#17161=CARTESIAN_POINT('Ctrl Pts',(92.6133947519263,1.80384167105459,-1.2664348540236));
#17162=CARTESIAN_POINT('Ctrl Pts',(92.6150448966668,1.82081775272028,-1.24203737307254));
#17163=CARTESIAN_POINT('Ctrl Pts',(92.6161946205806,1.8322621829349,-1.22509157070617));
#17164=CARTESIAN_POINT('Ctrl Pts',(92.6246065749992,1.91339688550704,-1.10127487111994));
#17165=CARTESIAN_POINT('Ctrl Pts',(92.6323010488496,1.97392167387891,-0.988697418926266));
#17166=CARTESIAN_POINT('Ctrl Pts',(92.6464846523659,2.06730213973287,-0.771795272521114));
#17167=CARTESIAN_POINT('Ctrl Pts',(92.652965112083,2.10281332490698,-0.669018632201595));
#17168=CARTESIAN_POINT('Ctrl Pts',(92.6627936131404,2.14636212546737,-0.504516092641967));
#17169=CARTESIAN_POINT('Ctrl Pts',(92.6662809413301,2.15961876363449,-0.444358752015239));
#17170=CARTESIAN_POINT('Ctrl Pts',(92.6708113377272,2.17387050670267,-0.363750332766872));
#17171=CARTESIAN_POINT('Ctrl Pts',(92.6719250188061,2.17712559513296,-0.343731677864219));
#17172=CARTESIAN_POINT('Ctrl Pts',(92.6737635189982,2.18208129385619,-0.310352238161295));
#17173=CARTESIAN_POINT('Ctrl Pts',(92.6744931859176,2.18393653878344,-0.297015976982417));
#17174=CARTESIAN_POINT('Ctrl Pts',(92.6759164668106,2.18733474312018,-0.270832292048455));
#17175=CARTESIAN_POINT('Ctrl Pts',(92.6766103474876,2.1888870024233,-0.257986645701906));
#17176=CARTESIAN_POINT('Ctrl Pts',(92.6782752408913,2.19235753304524,-0.226975919143379));
#17177=CARTESIAN_POINT('Ctrl Pts',(92.6792426845291,2.19416330339933,-0.208799055321895));
#17178=CARTESIAN_POINT('Ctrl Pts',(92.6824448665742,2.19942898908688,-0.148137968185167));
#17179=CARTESIAN_POINT('Ctrl Pts',(92.6846483395663,2.2018826010158,-0.105574880363342));
#17180=CARTESIAN_POINT('Ctrl Pts',(92.6953295990619,2.20787385170795,0.104053105674433));
#17181=CARTESIAN_POINT('Ctrl Pts',(92.7032559255081,2.19364040370517,0.271067532739719));
#17182=CARTESIAN_POINT('Ctrl Pts',(92.7158806168465,2.14242445694557,0.525533394984517));
#17183=CARTESIAN_POINT('Ctrl Pts',(92.7204396682846,2.11849156300855,0.614945750728927));
#17184=CARTESIAN_POINT('Ctrl Pts',(92.726331656623,2.08245227150757,0.722102984280509));
#17185=CARTESIAN_POINT('Ctrl Pts',(92.7274177064101,2.07561378465311,0.741530538680626));
#17186=CARTESIAN_POINT('Ctrl Pts',(92.7290213738526,2.0652588807805,0.769681840633855));
#17187=CARTESIAN_POINT('Ctrl Pts',(92.7295271010154,2.06195710450873,0.778483958151378));
#17188=CARTESIAN_POINT('Ctrl Pts',(92.7304212743774,2.05605879659927,0.793907302540494));
#17189=CARTESIAN_POINT('Ctrl Pts',(92.7308082972785,2.05348638546817,0.800537471534418));
#17190=CARTESIAN_POINT('Ctrl Pts',(92.7316579192573,2.04779767194742,0.814991790290467));
#17191=CARTESIAN_POINT('Ctrl Pts',(92.73212124037,2.04466864826521,0.82281045049415));
#17192=CARTESIAN_POINT('Ctrl Pts',(92.7334266378054,2.03577530029283,0.844668730947752));
#17193=CARTESIAN_POINT('Ctrl Pts',(92.7342743595535,2.02991076175273,0.858666763991459));
#17194=CARTESIAN_POINT('Ctrl Pts',(92.7402484158178,1.98792546895196,0.956046854019381));
#17195=CARTESIAN_POINT('Ctrl Pts',(92.7456178323101,1.94682567532868,1.0371788550614));
#17196=CARTESIAN_POINT('Ctrl Pts',(92.7524115566793,1.88933611209746,1.13513954124702));
#17197=CARTESIAN_POINT('Ctrl Pts',(92.7537750576747,1.87752821808702,1.15456506907185));
#17198=CARTESIAN_POINT('Ctrl Pts',(92.7604333567593,1.81847249629876,1.24841703644602));
#17199=CARTESIAN_POINT('Ctrl Pts',(92.7657382384729,1.76708684015812,1.32014868740261));
#17200=CARTESIAN_POINT('Ctrl Pts',(92.7747892184596,1.67052047249218,1.43917213770966));
#17201=CARTESIAN_POINT('Ctrl Pts',(92.7785769157666,1.62727698152837,1.48789307032024));
#17202=CARTESIAN_POINT('Ctrl Pts',(92.7847978182065,1.55118258533804,1.56633311745049));
#17203=CARTESIAN_POINT('Ctrl Pts',(92.7872737206403,1.51948099481991,1.59710511500307));
#17204=CARTESIAN_POINT('Ctrl Pts',(92.7907005704363,1.47359114764053,1.63904513347379));
#17205=CARTESIAN_POINT('Ctrl Pts',(92.7916856117272,1.46015950912441,1.6510221243255));
#17206=CARTESIAN_POINT('Ctrl Pts',(92.7933714842882,1.43675916087808,1.67137926254787));
#17207=CARTESIAN_POINT('Ctrl Pts',(92.7940755631496,1.42686024185909,1.67983790468767));
#17208=CARTESIAN_POINT('Ctrl Pts',(92.7955061254174,1.40649193239773,1.6969327063139));
#17209=CARTESIAN_POINT('Ctrl Pts',(92.796232266774,1.39601655870108,1.7055608886279));
#17210=CARTESIAN_POINT('Ctrl Pts',(92.7980611003176,1.36929206435639,1.72716169733097));
#17211=CARTESIAN_POINT('Ctrl Pts',(92.7991584857871,1.35293765204394,1.74000230895858));
#17212=CARTESIAN_POINT('Ctrl Pts',(92.8034198971075,1.28821659860586,1.78935353665396));
#17213=CARTESIAN_POINT('Ctrl Pts',(92.8065156126625,1.23853250913716,1.82409597482429));
#17214=CARTESIAN_POINT('Ctrl Pts',(92.8170834000714,1.0609482574718,1.93766931496357));
#17215=CARTESIAN_POINT('Ctrl Pts',(92.8242035545896,0.92648391386854,2.00544295858634));
#17216=CARTESIAN_POINT('Ctrl Pts',(92.8361302074394,0.697959112408725,2.09269797525605));
#17217=CARTESIAN_POINT('Ctrl Pts',(92.8408111338332,0.607682531550858,2.12067207029121));
#17218=CARTESIAN_POINT('Ctrl Pts',(92.8465790745721,0.50119742658519,2.14630982798855));
#17219=CARTESIAN_POINT('Ctrl Pts',(92.8473828885217,0.486457857147284,2.14969845937399));
#17220=CARTESIAN_POINT('Ctrl Pts',(92.8486416764787,0.463558845433109,2.15471538740191));
#17221=CARTESIAN_POINT('Ctrl Pts',(92.8490908725455,0.45542282106395,2.15644968717707));
#17222=CARTESIAN_POINT('Ctrl Pts',(92.849933637424,0.440229947525869,2.15959843301897));
#17223=CARTESIAN_POINT('Ctrl Pts',(92.8503265557052,0.433175763365217,2.1610244217896));
#17224=CARTESIAN_POINT('Ctrl Pts',(92.8512392542547,0.416855141835998,2.16424048130748));
#17225=CARTESIAN_POINT('Ctrl Pts',(92.8517604018492,0.407584055186156,2.16600560975387));
#17226=CARTESIAN_POINT('Ctrl Pts',(92.8534268139649,0.378079127532255,2.17142693846586));
#17227=CARTESIAN_POINT('Ctrl Pts',(92.8545835735802,0.357805879830048,2.17485945896453));
#17228=CARTESIAN_POINT('Ctrl Pts',(92.86214101456,0.2264544342756,2.19521273006672));
#17229=CARTESIAN_POINT('Ctrl Pts',(92.8688761504706,0.11427588574401,2.20390054763915));
#17230=CARTESIAN_POINT('Ctrl Pts',(92.875663664803,0.00128964400580923,
2.20399971703118));
#17231=CARTESIAN_POINT('Ctrl Pts',(92.8757024023764,0.000644818249044074,
2.20399999999996));
#17232=CARTESIAN_POINT('Ctrl Pts',(92.8757411398941,1.22339489286472E-10,
2.204));
#17233=CARTESIAN_POINT('Origin',(66.9212607628943,0.,0.));
#17234=CARTESIAN_POINT('',(93.7322127872898,-1.52555169845894E-15,2.204));
#17235=CARTESIAN_POINT('',(93.6281258142613,1.15214847468432E-14,2.204));
#17236=CARTESIAN_POINT('',(66.9212607628943,-2.69912154532077E-16,2.204));
#17237=CARTESIAN_POINT('',(93.7322042748184,0.000170073928470324,2.20399969046683));
#17238=CARTESIAN_POINT('Ctrl Pts',(93.7322127872898,-1.52555169845894E-15,
2.204));
#17239=CARTESIAN_POINT('Ctrl Pts',(93.7322097718937,5.67412332685096E-5,
2.204));
#17240=CARTESIAN_POINT('Ctrl Pts',(93.732206756565,0.000113482473413851,
2.20399999780882));
#17241=CARTESIAN_POINT('Ctrl Pts',(93.7322037413037,0.000170223720302068,
2.20399999342647));
#17242=CARTESIAN_POINT('Ctrl Pts',(93.7322037507425,0.000170046101699417,
2.20399999344018));
#17243=CARTESIAN_POINT('Ctrl Pts',(93.7311627020912,0.019760519554234,2.20399848196847));
#17244=CARTESIAN_POINT('Ctrl Pts',(93.7301297689015,0.0393505287422103,
2.20373577308858));
#17245=CARTESIAN_POINT('Ctrl Pts',(93.7273906911225,0.0916756679353474,
2.20233610000477));
#17246=CARTESIAN_POINT('Ctrl Pts',(93.7256988646687,0.12439382954957,2.20073056969929));
#17247=CARTESIAN_POINT('Ctrl Pts',(93.7141567735045,0.349874654399729,2.18462101571674));
#17248=CARTESIAN_POINT('Ctrl Pts',(93.7051076533056,0.540019923774952,2.14554366317177));
#17249=CARTESIAN_POINT('Ctrl Pts',(93.6929682032714,0.773520450323089,2.06450571506348));
#17250=CARTESIAN_POINT('Ctrl Pts',(93.6902857141559,0.823743286802514,2.04498511298578));
#17251=CARTESIAN_POINT('Ctrl Pts',(93.6864030017052,0.893345757848016,2.01495183127093));
#17252=CARTESIAN_POINT('Ctrl Pts',(93.6852665889057,0.913362168797062,2.00595787864736));
#17253=CARTESIAN_POINT('Ctrl Pts',(93.6832358187998,0.948413873538154,1.98957474364813));
#17254=CARTESIAN_POINT('Ctrl Pts',(93.6823478957235,0.963505675530331,1.98231009576007));
#17255=CARTESIAN_POINT('Ctrl Pts',(93.6809884392729,0.986224756900104,1.97105322225954));
#17256=CARTESIAN_POINT('Ctrl Pts',(93.6805243255696,0.993914174789823,1.96718699776744));
#17257=CARTESIAN_POINT('Ctrl Pts',(93.679673151206,1.00788950253193,1.96005737457327));
#17258=CARTESIAN_POINT('Ctrl Pts',(93.6792869892997,1.01418256100026,1.95680859827848));
#17259=CARTESIAN_POINT('Ctrl Pts',(93.6784067901617,1.02842008709858,1.94937138051269));
#17260=CARTESIAN_POINT('Ctrl Pts',(93.6779116424099,1.03635464206135,1.94516469862781));
#17261=CARTESIAN_POINT('Ctrl Pts',(93.6763801141125,1.06067715312717,1.93207851481566));
#17262=CARTESIAN_POINT('Ctrl Pts',(93.6753344342274,1.07697795162622,1.92303974356451));
#17263=CARTESIAN_POINT('Ctrl Pts',(93.6656452355125,1.22546184882725,1.8382256234807));
#17264=CARTESIAN_POINT('Ctrl Pts',(93.656373714362,1.34956102328693,1.74914557214675));
#17265=CARTESIAN_POINT('Ctrl Pts',(93.6401175890809,1.55251973689422,1.56891067381643));
#17266=CARTESIAN_POINT('Ctrl Pts',(93.6330965682512,1.63501923341314,1.4827395436678));
#17267=CARTESIAN_POINT('Ctrl Pts',(93.6242513395088,1.73370478225863,1.36135116094821));
#17268=CARTESIAN_POINT('Ctrl Pts',(93.6221689880822,1.75651212768382,1.33179376797084));
#17269=CARTESIAN_POINT('Ctrl Pts',(93.6191934608053,1.78846544041769,1.28813382031447));
#17270=CARTESIAN_POINT('Ctrl Pts',(93.618276937348,1.79821746453001,1.27448473620757));
#17271=CARTESIAN_POINT('Ctrl Pts',(93.6166757904982,1.81509062968977,1.25028951781281));
#17272=CARTESIAN_POINT('Ctrl Pts',(93.6159886556115,1.8222779508952,1.23979068858649));
#17273=CARTESIAN_POINT('Ctrl Pts',(93.6145626135252,1.83707876191197,1.21776371347906));
#17274=CARTESIAN_POINT('Ctrl Pts',(93.6138243531795,1.844675599282,1.20622501410989));
#17275=CARTESIAN_POINT('Ctrl Pts',(93.6119015160732,1.86428448747864,1.17582287273593));
#17276=CARTESIAN_POINT('Ctrl Pts',(93.6107235384816,1.87611896963305,1.15684646285209));
#17277=CARTESIAN_POINT('Ctrl Pts',(93.6055521900641,1.92723226181816,1.07203915008598));
#17278=CARTESIAN_POINT('Ctrl Pts',(93.6016727659889,1.96335155688039,1.0043626424015));
#17279=CARTESIAN_POINT('Ctrl Pts',(93.5909362786264,2.05523820865861,0.808205881616465));
#17280=CARTESIAN_POINT('Ctrl Pts',(93.584305774443,2.10239637081351,0.676113590212933));
#17281=CARTESIAN_POINT('Ctrl Pts',(93.5735931051871,2.15606209240247,0.463939127097435));
#17282=CARTESIAN_POINT('Ctrl Pts',(93.569662693869,2.17128802660668,0.386457545033741));
#17283=CARTESIAN_POINT('Ctrl Pts',(93.5645432732366,2.18499300103845,0.289456487168083));
#17284=CARTESIAN_POINT('Ctrl Pts',(93.5635358915841,2.18741499916114,0.270545829009715));
#17285=CARTESIAN_POINT('Ctrl Pts',(93.5620305713203,2.19062582557879,0.242603824419862));
#17286=CARTESIAN_POINT('Ctrl Pts',(93.5615426502332,2.19160480323373,0.233594742868918));
#17287=CARTESIAN_POINT('Ctrl Pts',(93.5607044760275,2.19318099568821,0.218206704199088));
#17288=CARTESIAN_POINT('Ctrl Pts',(93.5603557754096,2.1938059986527,0.211830792826221));
#17289=CARTESIAN_POINT('Ctrl Pts',(93.559554746513,2.19517163778844,0.197244604355678));
#17290=CARTESIAN_POINT('Ctrl Pts',(93.5591014332354,2.19589400251204,0.189033008989035));
#17291=CARTESIAN_POINT('Ctrl Pts',(93.5578383982255,2.1977682051405,0.16626522721368));
#17292=CARTESIAN_POINT('Ctrl Pts',(93.5570235145801,2.19882145880143,0.151701609389933));
#17293=CARTESIAN_POINT('Ctrl Pts',(93.552132572279,2.20422920517113,0.0649542351037719));
#17294=CARTESIAN_POINT('Ctrl Pts',(93.5479018377236,2.20517322976083,-0.00739231330563989));
#17295=CARTESIAN_POINT('Ctrl Pts',(93.535693768828,2.19774872551549,-0.212708820541933));
#17296=CARTESIAN_POINT('Ctrl Pts',(93.5276005580955,2.18088843175286,-0.345069445179283));
#17297=CARTESIAN_POINT('Ctrl Pts',(93.5159931108789,2.13846789426629,-0.537233741348164));
#17298=CARTESIAN_POINT('Ctrl Pts',(93.5122957336523,2.12206607826796,-0.59875002906928));
#17299=CARTESIAN_POINT('Ctrl Pts',(93.5062086403788,2.09004364066282,-0.700867662469533));
#17300=CARTESIAN_POINT('Ctrl Pts',(93.5037783362893,2.07584349521482,-0.741870647308984));
#17301=CARTESIAN_POINT('Ctrl Pts',(93.5004084762503,2.05413388652524,-0.799040470477603));
#17302=CARTESIAN_POINT('Ctrl Pts',(93.4994360893055,2.04762545585654,-0.815574469852261));
#17303=CARTESIAN_POINT('Ctrl Pts',(93.4977703241192,2.03605470230212,-0.843956863833963));
#17304=CARTESIAN_POINT('Ctrl Pts',(93.497073793507,2.0310871902943,-0.855842727409971));
#17305=CARTESIAN_POINT('Ctrl Pts',(93.4957432895972,2.02135044406547,-0.878577718898446));
#17306=CARTESIAN_POINT('Ctrl Pts',(93.4951087968149,2.01659736757408,-0.889433241179307));
#17307=CARTESIAN_POINT('Ctrl Pts',(93.4934502120683,2.00388510223251,-0.91784089035594));
#17308=CARTESIAN_POINT('Ctrl Pts',(93.4924310556804,1.99578275706997,-0.935328082015062));
#17309=CARTESIAN_POINT('Ctrl Pts',(93.4888037306351,1.96591043233258,-0.997645038404249));
#17310=CARTESIAN_POINT('Ctrl Pts',(93.4862400619051,1.94285013870369,-1.04184128696349));
#17311=CARTESIAN_POINT('Ctrl Pts',(93.4756156453453,1.83944885091134,-1.22462056636108));
#17312=CARTESIAN_POINT('Ctrl Pts',(93.4680215633989,1.74563093271669,-1.35500604578568));
#17313=CARTESIAN_POINT('Ctrl Pts',(93.4558335291167,1.57819061843789,-1.54112432022936));
#17314=CARTESIAN_POINT('Ctrl Pts',(93.4513794049857,1.51381811716872,-1.60440068541811));
#17315=CARTESIAN_POINT('Ctrl Pts',(93.4456197649533,1.43044968978261,-1.67685450544111));
#17316=CARTESIAN_POINT('Ctrl Pts',(93.4445498100754,1.41495894746829,-1.68994629108733));
#17317=CARTESIAN_POINT('Ctrl Pts',(93.4429685609006,1.39211372736261,-1.70871930162054));
#17318=CARTESIAN_POINT('Ctrl Pts',(93.4424687908163,1.38490007930343,-1.7145710967179));
#17319=CARTESIAN_POINT('Ctrl Pts',(93.4415811297548,1.37210578412407,-1.72481655915851));
#17320=CARTESIAN_POINT('Ctrl Pts',(93.4411945882044,1.36654058716386,-1.72922909635091));
#17321=CARTESIAN_POINT('Ctrl Pts',(93.4403483645369,1.35437213683413,-1.73878179600393));
#17322=CARTESIAN_POINT('Ctrl Pts',(93.4398879893912,1.34776100335565,-1.74391120537744));
#17323=CARTESIAN_POINT('Ctrl Pts',(93.4385866098392,1.32909212030213,-1.75822635141928));
#17324=CARTESIAN_POINT('Ctrl Pts',(93.4377399480984,1.31696880891075,-1.76732535133342));
#17325=CARTESIAN_POINT('Ctrl Pts',(93.4313594392685,1.2256856373801,-1.8343760190016));
#17326=CARTESIAN_POINT('Ctrl Pts',(93.4255421403649,1.14283576217411,-1.8871045203934));
#17327=CARTESIAN_POINT('Ctrl Pts',(93.4187993255949,1.04407012779767,-1.94106739643301));
#17328=CARTESIAN_POINT('Ctrl Pts',(93.417931811131,1.03131346971472,-1.94787514827089));
#17329=CARTESIAN_POINT('Ctrl Pts',(93.4118035554381,0.940796389506141,-1.99504226607016));
#17330=CARTESIAN_POINT('Ctrl Pts',(93.4065302328044,0.860754130648719,-2.0308606299483));
#17331=CARTESIAN_POINT('Ctrl Pts',(93.3974401910949,0.716851736606003,-2.08521540943635));
#17332=CARTESIAN_POINT('Ctrl Pts',(93.3935858656735,0.653887000898354,-2.10580925731379));
#17333=CARTESIAN_POINT('Ctrl Pts',(93.3880844748785,0.560802004611938,-2.13167560901881));
#17334=CARTESIAN_POINT('Ctrl Pts',(93.3863717034813,0.5313515489001,-2.13920673355858));
#17335=CARTESIAN_POINT('Ctrl Pts',(93.3832932872548,0.477556646441944,-2.15178371348094));
#17336=CARTESIAN_POINT('Ctrl Pts',(93.3819215387299,0.453265002794533,-2.15703138799492));
#17337=CARTESIAN_POINT('Ctrl Pts',(93.3797784423691,0.414815566812925,-2.16465930452163));
#17338=CARTESIAN_POINT('Ctrl Pts',(93.3789984184152,0.400714900514885,-2.16731387697486));
#17339=CARTESIAN_POINT('Ctrl Pts',(93.3775411243086,0.374175172314,-2.17204234241065));
#17340=CARTESIAN_POINT('Ctrl Pts',(93.3768628847,0.361742341462967,-2.17414753049789));
#17341=CARTESIAN_POINT('Ctrl Pts',(93.3753424389276,0.333692710915717,-2.17864976073448));
#17342=CARTESIAN_POINT('Ctrl Pts',(93.374502193898,0.318066740350762,-2.18098582562306));
#17343=CARTESIAN_POINT('Ctrl Pts',(93.3720319982808,0.271773201860081,-2.18739853947103));
#17344=CARTESIAN_POINT('Ctrl Pts',(93.3704170353733,0.241042795640048,-2.1909978407837));
#17345=CARTESIAN_POINT('Ctrl Pts',(93.3615010376657,0.0690644453104937,
-2.20747849572024));
#17346=CARTESIAN_POINT('Ctrl Pts',(93.3546168788456,-0.0730955019596106,
-2.20734976347764));
#17347=CARTESIAN_POINT('Ctrl Pts',(93.3428687953956,-0.315007155167834,
-2.18371967773079));
#17348=CARTESIAN_POINT('Ctrl Pts',(93.3379961410825,-0.414942724344834,
-2.1669520831745));
#17349=CARTESIAN_POINT('Ctrl Pts',(93.3312896607526,-0.544514657835592,
-2.13591800035786));
#17350=CARTESIAN_POINT('Ctrl Pts',(93.3296556287795,-0.575495998444965,
-2.1277796176765));
#17351=CARTESIAN_POINT('Ctrl Pts',(93.3268317334739,-0.627738776872336,
-2.11283171363186));
#17352=CARTESIAN_POINT('Ctrl Pts',(93.3256576586665,-0.64909466298474,-2.10636888155922));
#17353=CARTESIAN_POINT('Ctrl Pts',(93.323950770794,-0.679538917234773,-2.09664874151746));
#17354=CARTESIAN_POINT('Ctrl Pts',(93.323432213196,-0.688710363921782,-2.09365400985207));
#17355=CARTESIAN_POINT('Ctrl Pts',(93.3225237070262,-0.704636047269229,
-2.08833786697613));
#17356=CARTESIAN_POINT('Ctrl Pts',(93.3221353410121,-0.711399117455989,
-2.08604369573591));
#17357=CARTESIAN_POINT('Ctrl Pts',(93.3212998403101,-0.725850661122635,
-2.08106298377712));
#17358=CARTESIAN_POINT('Ctrl Pts',(93.3208521734447,-0.733535305931576,
-2.07836673262028));
#17359=CARTESIAN_POINT('Ctrl Pts',(93.3196195223198,-0.754541459795169,
-2.07086545587906));
#17360=CARTESIAN_POINT('Ctrl Pts',(93.3188297545146,-0.767831653917365,
-2.06597460796911));
#17361=CARTESIAN_POINT('Ctrl Pts',(93.314435656475,-0.840915228423101,-2.03827695988927));
#17362=CARTESIAN_POINT('Ctrl Pts',(93.3107099447663,-0.899736185700069,
-2.01300393242826));
#17363=CARTESIAN_POINT('Ctrl Pts',(93.2990784541018,-1.07678419263712,-1.92762240560806));
#17364=CARTESIAN_POINT('Ctrl Pts',(93.2910132719407,-1.19076032610242,-1.85937729747585));
#17365=CARTESIAN_POINT('Ctrl Pts',(93.2769668415769,-1.38244641178254,-1.71970842838357));
#17366=CARTESIAN_POINT('Ctrl Pts',(93.2709184566932,-1.46249425211976,-1.65217145255705));
#17367=CARTESIAN_POINT('Ctrl Pts',(93.2637950308372,-1.55426712177235,-1.56282453194235));
#17368=CARTESIAN_POINT('Ctrl Pts',(93.2625013423239,-1.57082098966639,-1.54618507367729));
#17369=CARTESIAN_POINT('Ctrl Pts',(93.2604517607318,-1.59685685049937,-1.51916479257714));
#17370=CARTESIAN_POINT('Ctrl Pts',(93.2596884186271,-1.60651045926708,-1.5089524926651));
#17371=CARTESIAN_POINT('Ctrl Pts',(93.2582453923524,-1.62467398921813,-1.48936586950855));
#17372=CARTESIAN_POINT('Ctrl Pts',(93.2575649442616,-1.63320206381848,-1.48000922041482));
#17373=CARTESIAN_POINT('Ctrl Pts',(93.2560167234031,-1.65251777404208,-1.45844655054329));
#17374=CARTESIAN_POINT('Ctrl Pts',(93.2551512196613,-1.66325172373511,-1.44619329865406));
#17375=CARTESIAN_POINT('Ctrl Pts',(93.2528882395337,-1.69113650233488,-1.41364050494546));
#17376=CARTESIAN_POINT('Ctrl Pts',(93.2515000856677,-1.70805800766838,-1.39314753994207));
#17377=CARTESIAN_POINT('Ctrl Pts',(93.2411677876472,-1.83244648445708,-1.23683132560324));
#17378=CARTESIAN_POINT('Ctrl Pts',(93.2328909531915,-1.92393698612088,-1.08907436591619));
#17379=CARTESIAN_POINT('Ctrl Pts',(93.2188948834625,-2.0461212632412,-0.827278599629718));
#17380=CARTESIAN_POINT('Ctrl Pts',(93.213241039844,-2.08671590481652,-0.718757789847149));
#17381=CARTESIAN_POINT('Ctrl Pts',(93.2063432391737,-2.12284413955009,-0.59277777263816));
#17382=CARTESIAN_POINT('Ctrl Pts',(93.2055258691251,-2.12693042648767,-0.577944342532827));
#17383=CARTESIAN_POINT('Ctrl Pts',(93.2042530940948,-2.13298756204755,-0.555021936602559));
#17384=CARTESIAN_POINT('Ctrl Pts',(93.2038037445118,-2.13506851688171,-0.546962259726661));
#17385=CARTESIAN_POINT('Ctrl Pts',(93.2029657499129,-2.13884179796295,-0.531998396465917));
#17386=CARTESIAN_POINT('Ctrl Pts',(93.2025778074699,-2.14054643651055,-0.525097590067583));
#17387=CARTESIAN_POINT('Ctrl Pts',(93.2016835994286,-2.14437969618979,-0.509250704921521));
#17388=CARTESIAN_POINT('Ctrl Pts',(93.2011760872183,-2.1464857375539,-0.500299444509844));
#17389=CARTESIAN_POINT('Ctrl Pts',(93.1995380337278,-2.1530639224646,-0.471534035110906));
#17390=CARTESIAN_POINT('Ctrl Pts',(93.198396141276,-2.1573180629117,-0.451671690448005));
#17391=CARTESIAN_POINT('Ctrl Pts',(93.1899264316195,-2.18652268988393,-0.305477674139943));
#17392=CARTESIAN_POINT('Ctrl Pts',(93.1821573063825,-2.20063138225343,-0.177242546286337));
#17393=CARTESIAN_POINT('Ctrl Pts',(93.167932121181,-2.20584571300854,0.0595563532546467));
#17394=CARTESIAN_POINT('Ctrl Pts',(93.1614825328575,-2.20027104367885,0.167670236967142));
#17395=CARTESIAN_POINT('Ctrl Pts',(93.1528696039071,-2.18166274314294,0.315671461516062));
#17396=CARTESIAN_POINT('Ctrl Pts',(93.1505296893733,-2.17540539313061,0.356247769589945));
#17397=CARTESIAN_POINT('Ctrl Pts',(93.1464618591503,-2.1623740217958,0.427478953036301));
#17398=CARTESIAN_POINT('Ctrl Pts',(93.1447202327652,-2.15607183920648,0.458207412149979));
#17399=CARTESIAN_POINT('Ctrl Pts',(93.1421391995641,-2.14563863696147,0.504080004448933));
#17400=CARTESIAN_POINT('Ctrl Pts',(93.1412842698145,-2.14199847635309,0.519330681283016));
#17401=CARTESIAN_POINT('Ctrl Pts',(93.1397579948813,-2.13516798153441,0.546653041571861));
#17402=CARTESIAN_POINT('Ctrl Pts',(93.1390847639393,-2.1320372449889,0.558738804945016));
#17403=CARTESIAN_POINT('Ctrl Pts',(93.1376426961688,-2.12507735132605,0.584695907567733));
#17404=CARTESIAN_POINT('Ctrl Pts',(93.1368749799027,-2.12121468308368,0.598557712449143));
#17405=CARTESIAN_POINT('Ctrl Pts',(93.1348171178863,-2.11043685429857,0.635820461420807));
#17406=CARTESIAN_POINT('Ctrl Pts',(93.1335352379196,-2.10326828908577,0.659146373501317));
#17407=CARTESIAN_POINT('Ctrl Pts',(93.1255419100495,-2.05572260372239,0.805174479322779));
#17408=CARTESIAN_POINT('Ctrl Pts',(93.1191858336827,-2.0050102952646,0.924251044399654));
#17409=CARTESIAN_POINT('Ctrl Pts',(93.1083680505205,-1.89989264625379,1.12109443119273));
#17410=CARTESIAN_POINT('Ctrl Pts',(93.1038675718405,-1.85037762538199,1.20106058578348));
#17411=CARTESIAN_POINT('Ctrl Pts',(93.0967253368166,-1.76627647760122,1.31927901568861));
#17412=CARTESIAN_POINT('Ctrl Pts',(93.0941727973656,-1.73520146269131,1.35989155913785));
#17413=CARTESIAN_POINT('Ctrl Pts',(93.0899508911615,-1.68294317982559,1.42347843327447));
#17414=CARTESIAN_POINT('Ctrl Pts',(93.0883256849407,-1.66263377066695,1.44714800522346));
#17415=CARTESIAN_POINT('Ctrl Pts',(93.0860830128931,-1.63450566642378,1.4785559713312));
#17416=CARTESIAN_POINT('Ctrl Pts',(93.0854949148979,-1.62712041512728,1.48667941349272));
#17417=CARTESIAN_POINT('Ctrl Pts',(93.0845044803561,-1.6146758384688,1.5001640812214));
#17418=CARTESIAN_POINT('Ctrl Pts',(93.0841046020389,-1.60964964325076,1.50555583029049));
#17419=CARTESIAN_POINT('Ctrl Pts',(93.083287063713,-1.59937309601679,1.5164695039171));
#17420=CARTESIAN_POINT('Ctrl Pts',(93.0828692816428,-1.59412101086154,1.52198957147081));
#17421=CARTESIAN_POINT('Ctrl Pts',(93.0817803249256,-1.58042658569946,1.53623409562788));
#17422=CARTESIAN_POINT('Ctrl Pts',(93.081105912289,-1.57194070579182,1.54491611198152));
#17423=CARTESIAN_POINT('Ctrl Pts',(93.0783226559348,-1.536879475061,1.58019978883584));
#17424=CARTESIAN_POINT('Ctrl Pts',(93.076172509658,-1.50969848706039,1.606188045857));
#17425=CARTESIAN_POINT('Ctrl Pts',(93.0662158840075,-1.38271826954793,1.72152468665409));
#17426=CARTESIAN_POINT('Ctrl Pts',(93.0580726356368,-1.27556907243249,1.80235371970612));
#17427=CARTESIAN_POINT('Ctrl Pts',(93.0421788952118,-1.04964884311135,1.94248669645377));
#17428=CARTESIAN_POINT('Ctrl Pts',(93.0344589440366,-0.931519404037495,
2.00182368578717));
#17429=CARTESIAN_POINT('Ctrl Pts',(93.0257473730472,-0.786012160526536,
2.05922308164554));
#17430=CARTESIAN_POINT('Ctrl Pts',(93.0243970585048,-0.763099991436265,
2.06782332120856));
#17431=CARTESIAN_POINT('Ctrl Pts',(93.0222796121493,-0.726610012583107,
2.08083094843863));
#17432=CARTESIAN_POINT('Ctrl Pts',(93.0215041486329,-0.713124942137394,
2.08549091983997));
#17433=CARTESIAN_POINT('Ctrl Pts',(93.0200508900681,-0.687627510470923,
2.09402571236726));
#17434=CARTESIAN_POINT('Ctrl Pts',(93.0193721807329,-0.675625319625622,
2.09792891059018));
#17435=CARTESIAN_POINT('Ctrl Pts',(93.0178448045262,-0.648406158697861,
2.10652296177654));
#17436=CARTESIAN_POINT('Ctrl Pts',(93.0169981765061,-0.633170463847152,
2.11115246177686));
#17437=CARTESIAN_POINT('Ctrl Pts',(93.0148189473012,-0.593581853252356,
2.12271468697768));
#17438=CARTESIAN_POINT('Ctrl Pts',(93.0134945532719,-0.569156929815739,
2.12939369696192));
#17439=CARTESIAN_POINT('Ctrl Pts',(93.0026658215889,-0.366637333641922,
2.18103911231749));
#17440=CARTESIAN_POINT('Ctrl Pts',(92.9939307301204,-0.183686324100655,
2.20399999999957));
#17441=CARTESIAN_POINT('Ctrl Pts',(92.9850149380438,-5.17478421224737E-12,
2.204));
#17442=CARTESIAN_POINT('',(93.628116692315,0.00015915216883437,2.20399968871531));
#17443=CARTESIAN_POINT('Ctrl Pts',(92.8757411398941,1.22336862862227E-10,
2.204));
#17444=CARTESIAN_POINT('Ctrl Pts',(92.8857120941664,-0.16597480764464,2.20400000000921));
#17445=CARTESIAN_POINT('Ctrl Pts',(92.8956194489081,-0.331447695365568,
2.18525149933953));
#17446=CARTESIAN_POINT('Ctrl Pts',(92.9064630876008,-0.519824247182944,
2.141994705664));
#17447=CARTESIAN_POINT('Ctrl Pts',(92.9079766238444,-0.546268501020775,
2.13540379919117));
#17448=CARTESIAN_POINT('Ctrl Pts',(92.9103754214465,-0.588412773391464,
2.12406569395616));
#17449=CARTESIAN_POINT('Ctrl Pts',(92.9112706107889,-0.60419324834365,2.11963091203957));
#17450=CARTESIAN_POINT('Ctrl Pts',(92.9128554496667,-0.632220121278324,
2.11141609502695));
#17451=CARTESIAN_POINT('Ctrl Pts',(92.9135472907579,-0.644485659369196,
2.10770454586058));
#17452=CARTESIAN_POINT('Ctrl Pts',(92.9149923108652,-0.670164686830281,
2.09968895652059));
#17453=CARTESIAN_POINT('Ctrl Pts',(92.9157447301723,-0.683570718555069,
2.09536285806611));
#17454=CARTESIAN_POINT('Ctrl Pts',(92.9177257893932,-0.718951746174243,
2.08356977300461));
#17455=CARTESIAN_POINT('Ctrl Pts',(92.9189471745916,-0.740852152386469,
2.07588360817131));
#17456=CARTESIAN_POINT('Ctrl Pts',(92.9252213309961,-0.853705175131841,
2.03426322008874));
#17457=CARTESIAN_POINT('Ctrl Pts',(92.9300830402856,-0.942468709037799,
1.99469166928737));
#17458=CARTESIAN_POINT('Ctrl Pts',(92.9414454245451,-1.14743133916119,1.88657001334687));
#17459=CARTESIAN_POINT('Ctrl Pts',(92.9478207661505,-1.26050877095401,1.81297007782795));
#17460=CARTESIAN_POINT('Ctrl Pts',(92.9578941885746,-1.42052702019115,1.68657020255177));
#17461=CARTESIAN_POINT('Ctrl Pts',(92.9613879837666,-1.47283449179674,1.64108896410067));
#17462=CARTESIAN_POINT('Ctrl Pts',(92.9658068764573,-1.53344195171914,1.5831563720421));
#17463=CARTESIAN_POINT('Ctrl Pts',(92.9665817098654,-1.54387472307975,1.57298414948275));
#17464=CARTESIAN_POINT('Ctrl Pts',(92.9678092227109,-1.56008051337731,1.55686654748618));
#17465=CARTESIAN_POINT('Ctrl Pts',(92.9682566946432,-1.56592234609977,1.55099060484699));
#17466=CARTESIAN_POINT('Ctrl Pts',(92.9690588178212,-1.57627368946636,1.54046072635729));
#17467=CARTESIAN_POINT('Ctrl Pts',(92.9694124590533,-1.58079599423231,1.53581965563095));
#17468=CARTESIAN_POINT('Ctrl Pts',(92.9702735160431,-1.59170787776845,1.52452194753349));
#17469=CARTESIAN_POINT('Ctrl Pts',(92.970782529509,-1.59807615177979,1.51784509865212));
#17470=CARTESIAN_POINT('Ctrl Pts',(92.9723850422269,-1.61787659038382,1.49682248847123));
#17471=CARTESIAN_POINT('Ctrl Pts',(92.9734889876174,-1.63115856856638,1.48233730753433));
#17472=CARTESIAN_POINT('Ctrl Pts',(92.979342532078,-1.69983889654991,1.40539445215957));
#17473=CARTESIAN_POINT('Ctrl Pts',(92.9842791451023,-1.75184513578168,1.34000826903958));
#17474=CARTESIAN_POINT('Ctrl Pts',(92.9977380762131,-1.88170995631609,1.15621233656285));
#17475=CARTESIAN_POINT('Ctrl Pts',(93.0063129910829,-1.95208377297054,1.03297359515815));
#17476=CARTESIAN_POINT('Ctrl Pts',(93.0186552514051,-2.03908990171498,0.839469083831763));
#17477=CARTESIAN_POINT('Ctrl Pts',(93.022675189293,-2.06492338595088,0.773749911333875));
#17478=CARTESIAN_POINT('Ctrl Pts',(93.027804626213,-2.09457535058681,0.686183949310435));
#17479=CARTESIAN_POINT('Ctrl Pts',(93.0290079742925,-2.10128137152249,0.665365281627181));
#17480=CARTESIAN_POINT('Ctrl Pts',(93.0309540023276,-2.11171153231198,0.631253378607787));
#17481=CARTESIAN_POINT('Ctrl Pts',(93.0317027514431,-2.11562251891809,0.618019249956476));
#17482=CARTESIAN_POINT('Ctrl Pts',(93.0331440623767,-2.12295097675411,0.592335869865602));
#17483=CARTESIAN_POINT('Ctrl Pts',(93.033837101633,-2.12638386242474,0.579891638035345));
#17484=CARTESIAN_POINT('Ctrl Pts',(93.0354520312484,-2.1341675652148,0.550676817690431));
#17485=CARTESIAN_POINT('Ctrl Pts',(93.0363710463525,-2.13843039218138,0.533883540504832));
#17486=CARTESIAN_POINT('Ctrl Pts',(93.0393900926016,-2.15187276131681,0.478181606696938));
#17487=CARTESIAN_POINT('Ctrl Pts',(93.0414626949808,-2.16019204570835,0.43907244732139));
#17488=CARTESIAN_POINT('Ctrl Pts',(93.0515179052008,-2.19587260884659,0.245615908689154));
#17489=CARTESIAN_POINT('Ctrl Pts',(93.0590123663761,-2.20777866280608,0.088883934548864));
#17490=CARTESIAN_POINT('Ctrl Pts',(93.0681402053485,-2.2019826996651,-0.0994572953099441));
#17491=CARTESIAN_POINT('Ctrl Pts',(93.0696793206099,-2.2003257201682,-0.131096288299875));
#17492=CARTESIAN_POINT('Ctrl Pts',(93.0753771539066,-2.19173527411179,-0.247156957431132));
#17493=CARTESIAN_POINT('Ctrl Pts',(93.0796024441038,-2.18061968012059,-0.331187458397588));
#17494=CARTESIAN_POINT('Ctrl Pts',(93.0848525857204,-2.16187321222613,-0.429122473933823));
#17495=CARTESIAN_POINT('Ctrl Pts',(93.0856511739632,-2.15889678012207,-0.443854200772686));
#17496=CARTESIAN_POINT('Ctrl Pts',(93.0869082236893,-2.1540246845498,-0.466759069331786));
#17497=CARTESIAN_POINT('Ctrl Pts',(93.0873610619256,-2.15223256758269,-0.474954040688606));
#17498=CARTESIAN_POINT('Ctrl Pts',(93.0882030613034,-2.14883364602683,-0.490082250295158));
#17499=CARTESIAN_POINT('Ctrl Pts',(93.0885914831957,-2.14723999215333,-0.497018170478371));
#17500=CARTESIAN_POINT('Ctrl Pts',(93.0895001550641,-2.14345199701084,-0.513146023942134));
#17501=CARTESIAN_POINT('Ctrl Pts',(93.0900218243079,-2.14123210605389,-0.522331663472147));
#17502=CARTESIAN_POINT('Ctrl Pts',(93.0917053729284,-2.13392121010454,-0.551753279874298));
#17503=CARTESIAN_POINT('Ctrl Pts',(93.0928791976697,-2.128602016111,-0.571930769480351));
#17504=CARTESIAN_POINT('Ctrl Pts',(93.0994784596318,-2.0974268406941,-0.683723981244553));
#17505=CARTESIAN_POINT('Ctrl Pts',(93.1051428419745,-2.06594449814274,-0.773658980374074));
#17506=CARTESIAN_POINT('Ctrl Pts',(93.1213703375746,-1.9602115676304,-1.02271678520752));
#17507=CARTESIAN_POINT('Ctrl Pts',(93.1319268447301,-1.8726323959279,-1.17543409313561));
#17508=CARTESIAN_POINT('Ctrl Pts',(93.1436393170979,-1.74870780052214,-1.34188887163963));
#17509=CARTESIAN_POINT('Ctrl Pts',(93.1454287471041,-1.72899446881725,-1.36719530218094));
#17510=CARTESIAN_POINT('Ctrl Pts',(93.1480850707039,-1.69855258364111,-1.40456221759031));
#17511=CARTESIAN_POINT('Ctrl Pts',(93.1489680547748,-1.68823311180229,-1.41694914594841));
#17512=CARTESIAN_POINT('Ctrl Pts',(93.1504944592617,-1.67004650090356,-1.43829859665395));
#17513=CARTESIAN_POINT('Ctrl Pts',(93.1511403577285,-1.66224091094551,-1.44731245076247));
#17514=CARTESIAN_POINT('Ctrl Pts',(93.1524869770361,-1.64573809871651,-1.46606019035062));
#17515=CARTESIAN_POINT('Ctrl Pts',(93.1531870710633,-1.63702676043598,-1.47578107015957));
#17516=CARTESIAN_POINT('Ctrl Pts',(93.1548535338255,-1.61597832709175,-1.49885305221158));
#17517=CARTESIAN_POINT('Ctrl Pts',(93.1558164635063,-1.60356130664935,-1.5121301491978));
#17518=CARTESIAN_POINT('Ctrl Pts',(93.1591591091192,-1.55958260866614,-1.55800405317259));
#17519=CARTESIAN_POINT('Ctrl Pts',(93.1615023337911,-1.52717894733907,-1.58977966251503));
#17520=CARTESIAN_POINT('Ctrl Pts',(93.1672486566337,-1.44407642941321,-1.66638396371345));
#17521=CARTESIAN_POINT('Ctrl Pts',(93.1706034339528,-1.39225038313005,-1.70992162082279));
#17522=CARTESIAN_POINT('Ctrl Pts',(93.1809051328467,-1.22496669804652,-1.83779618924647));
#17523=CARTESIAN_POINT('Ctrl Pts',(93.1876541138286,-1.10326762233292,-1.9133308267168));
#17524=CARTESIAN_POINT('Ctrl Pts',(93.1976269331511,-0.923886170119412,
-2.00182773612126));
#17525=CARTESIAN_POINT('Ctrl Pts',(93.2005346910079,-0.871691372103053,
-2.02510076458536));
#17526=CARTESIAN_POINT('Ctrl Pts',(93.2042894974147,-0.80565507687788,-2.05151942906736));
#17527=CARTESIAN_POINT('Ctrl Pts',(93.2050351179288,-0.792605402354965,
-2.05659639373236));
#17528=CARTESIAN_POINT('Ctrl Pts',(93.2062221063346,-0.771953443032062,
-2.0644052709607));
#17529=CARTESIAN_POINT('Ctrl Pts',(93.2066587072136,-0.764382784488698,
-2.06722040322442));
#17530=CARTESIAN_POINT('Ctrl Pts',(93.2074923943445,-0.749980234662113,
-2.07248602560038));
#17531=CARTESIAN_POINT('Ctrl Pts',(93.2078890133934,-0.74315150428437,-2.07494446063364));
#17532=CARTESIAN_POINT('Ctrl Pts',(93.2088397696507,-0.726834375344231,
-2.08072796802666));
#17533=CARTESIAN_POINT('Ctrl Pts',(93.209395688463,-0.717335192391652,-2.08402190483849));
#17534=CARTESIAN_POINT('Ctrl Pts',(93.2113128691234,-0.684703331373508,
-2.09508779563051));
#17535=CARTESIAN_POINT('Ctrl Pts',(93.2126909659544,-0.661465054762219,
-2.10254022648159));
#17536=CARTESIAN_POINT('Ctrl Pts',(93.2161473712218,-0.603573711328786,
-2.12005107776756));
#17537=CARTESIAN_POINT('Ctrl Pts',(93.2182445883708,-0.568788814842518,
-2.12964711603335));
#17538=CARTESIAN_POINT('Ctrl Pts',(93.2278740428796,-0.409835201308626,
-2.16932528321663));
#17539=CARTESIAN_POINT('Ctrl Pts',(93.2356412493696,-0.283430906475186,
-2.18943006685147));
#17540=CARTESIAN_POINT('Ctrl Pts',(93.2503756383045,-0.0367672624844075,
-2.20693260825921));
#17541=CARTESIAN_POINT('Ctrl Pts',(93.2573380813423,0.0829660686266078,
-2.20568060950862));
#17542=CARTESIAN_POINT('Ctrl Pts',(93.2653723495126,0.22658194354453,-2.19246093326515));
#17543=CARTESIAN_POINT('Ctrl Pts',(93.266733579356,0.251103262326049,-2.18978801314081));
#17544=CARTESIAN_POINT('Ctrl Pts',(93.2688690035628,0.289860627520369,-2.18490368869045));
#17545=CARTESIAN_POINT('Ctrl Pts',(93.2696516493694,0.304128222890052,-2.18296343307092));
#17546=CARTESIAN_POINT('Ctrl Pts',(93.2710501294238,0.329731242483727,-2.17922577918297));
#17547=CARTESIAN_POINT('Ctrl Pts',(93.2716675502865,0.341073486155282,-2.17747940814325));
#17548=CARTESIAN_POINT('Ctrl Pts',(93.273111674567,0.367689860460666,-2.17316820005079));
#17549=CARTESIAN_POINT('Ctrl Pts',(93.2739360472885,0.382951725101924,-2.1705307765781));
#17550=CARTESIAN_POINT('Ctrl Pts',(93.2763382617193,0.427610377305468,-2.1623275527504));
#17551=CARTESIAN_POINT('Ctrl Pts',(93.2779022030043,0.456923710815786,-2.1563237037659));
#17552=CARTESIAN_POINT('Ctrl Pts',(93.2850363591304,0.591532826864561,-2.1258852055745));
#17553=CARTESIAN_POINT('Ctrl Pts',(93.2903789607237,0.695068772461029,-2.0943212613889));
#17554=CARTESIAN_POINT('Ctrl Pts',(93.3040300853188,0.956866743701798,-1.99294407787394));
#17555=CARTESIAN_POINT('Ctrl Pts',(93.3121370744278,1.1099527124253,-1.91191264640855));
#17556=CARTESIAN_POINT('Ctrl Pts',(93.3221863635486,1.26849471930347,-1.80248135004072));
#17557=CARTESIAN_POINT('Ctrl Pts',(93.3232442162411,1.28483624019738,-1.79086952351595));
#17558=CARTESIAN_POINT('Ctrl Pts',(93.3248084498348,1.30844411100608,-1.77360499609327));
#17559=CARTESIAN_POINT('Ctrl Pts',(93.3253035782826,1.31583747567764,-1.76812680690075));
#17560=CARTESIAN_POINT('Ctrl Pts',(93.3261903484758,1.32893246731872,-1.75829631920462));
#17561=CARTESIAN_POINT('Ctrl Pts',(93.3265807397198,1.33464744900739,-1.75396226698755));
#17562=CARTESIAN_POINT('Ctrl Pts',(93.3274370442597,1.34707301772952,-1.74444323373215));
#17563=CARTESIAN_POINT('Ctrl Pts',(93.3279036828008,1.3537747774502,-1.73924746882646));
#17564=CARTESIAN_POINT('Ctrl Pts',(93.3292519455852,1.37294571020943,-1.72420662413077));
#17565=CARTESIAN_POINT('Ctrl Pts',(93.3301399516686,1.38533838603356,-1.71426542060749));
#17566=CARTESIAN_POINT('Ctrl Pts',(93.3380978143606,1.49445500458864,-1.62477793687495));
#17567=CARTESIAN_POINT('Ctrl Pts',(93.3456211912652,1.58433507152372,-1.53726254067326));
#17568=CARTESIAN_POINT('Ctrl Pts',(93.3628039862581,1.77153319192621,-1.32103731846744));
#17569=CARTESIAN_POINT('Ctrl Pts',(93.3723850219719,1.86317381736594,-1.18830466636839));
#17570=CARTESIAN_POINT('Ctrl Pts',(93.3829660220522,1.95269842699355,-1.02242355272343));
#17571=CARTESIAN_POINT('Ctrl Pts',(93.3845029364724,1.96537617711405,-0.997836483793361));
#17572=CARTESIAN_POINT('Ctrl Pts',(93.386931243176,1.9848755961537,-0.958205273341404));
#17573=CARTESIAN_POINT('Ctrl Pts',(93.3878329528898,1.9919965371105,-0.943312405903441));
#17574=CARTESIAN_POINT('Ctrl Pts',(93.3894252085864,2.00435383217488,-0.916704058621696));
#17575=CARTESIAN_POINT('Ctrl Pts',(93.3901180183246,2.009656394451,-0.90502033215498));
#17576=CARTESIAN_POINT('Ctrl Pts',(93.391560986075,2.0205423164275,-0.880466655891991));
#17577=CARTESIAN_POINT('Ctrl Pts',(93.3923104280041,2.02610544645255,-0.867588333794463));
#17578=CARTESIAN_POINT('Ctrl Pts',(93.3942743854889,2.04043971690847,-0.833515365448055));
#17579=CARTESIAN_POINT('Ctrl Pts',(93.3954818761748,2.04900372810589,-0.812235112041747));
#17580=CARTESIAN_POINT('Ctrl Pts',(93.4015121595105,2.09046864163244,-0.704369159062519));
#17581=CARTESIAN_POINT('Ctrl Pts',(93.4061622953983,2.11822193649965,-0.615900431620633));
#17582=CARTESIAN_POINT('Ctrl Pts',(93.4152255072159,2.16223272988468,-0.436797320582795));
#17583=CARTESIAN_POINT('Ctrl Pts',(93.4196320422737,2.17854750799947,-0.346371716055772));
#17584=CARTESIAN_POINT('Ctrl Pts',(93.4256251541043,2.19287200190162,-0.223488654935204));
#17585=CARTESIAN_POINT('Ctrl Pts',(93.4271760137457,2.19587853708624,-0.191708614386923));
#17586=CARTESIAN_POINT('Ctrl Pts',(93.4328686150059,2.20431113108033,-0.0757650251248282));
#17587=CARTESIAN_POINT('Ctrl Pts',(93.4370766342163,2.2055953601929,0.00861903260830226));
#17588=CARTESIAN_POINT('Ctrl Pts',(93.442307001207,2.20141010894884,0.107866189251395));
#17589=CARTESIAN_POINT('Ctrl Pts',(93.4431050707776,2.20062394606502,0.122864990971442));
#17590=CARTESIAN_POINT('Ctrl Pts',(93.4443614759056,2.19916002346551,0.146224225494058));
#17591=CARTESIAN_POINT('Ctrl Pts',(93.4448141974418,2.1985877120656,0.154591075306799));
#17592=CARTESIAN_POINT('Ctrl Pts',(93.4456561005437,2.19744145379142,0.170052087471947));
#17593=CARTESIAN_POINT('Ctrl Pts',(93.446044544474,2.19688087979474,0.177146974617733));
#17594=CARTESIAN_POINT('Ctrl Pts',(93.4469534285425,2.19549570431192,0.193659448176491));
#17595=CARTESIAN_POINT('Ctrl Pts',(93.447475290178,2.1946448666491,0.203074548105166));
#17596=CARTESIAN_POINT('Ctrl Pts',(93.4491600912566,2.19171998101012,0.233271779701937));
#17597=CARTESIAN_POINT('Ctrl Pts',(93.4503350000238,2.18941115014019,0.254029425706188));
#17598=CARTESIAN_POINT('Ctrl Pts',(93.4569463929965,2.17491710866893,0.369391188702525));
#17599=CARTESIAN_POINT('Ctrl Pts',(93.4626227131336,2.15689606184709,0.463152999278649));
#17600=CARTESIAN_POINT('Ctrl Pts',(93.4788964199204,2.08851564099992,0.725728379517686));
#17601=CARTESIAN_POINT('Ctrl Pts',(93.4894855774807,2.02392820326077,0.890119402739486));
#17602=CARTESIAN_POINT('Ctrl Pts',(93.5013926642765,1.92383579477993,1.07596546090861));
#17603=CARTESIAN_POINT('Ctrl Pts',(93.5033458877859,1.90647163138808,1.1064411219035));
#17604=CARTESIAN_POINT('Ctrl Pts',(93.5061783003804,1.87989367634389,1.15060290872919));
#17605=CARTESIAN_POINT('Ctrl Pts',(93.5070776292229,1.87124242880466,1.16461971534029));
#17606=CARTESIAN_POINT('Ctrl Pts',(93.5086650255563,1.85559564035487,1.18934620640933));
#17607=CARTESIAN_POINT('Ctrl Pts',(93.5093553538396,1.8486625397758,1.20009433081762));
#17608=CARTESIAN_POINT('Ctrl Pts',(93.5108041687347,1.83384164039406,1.22263737497164));
#17609=CARTESIAN_POINT('Ctrl Pts',(93.511561820532,1.82593268975664,1.23441773240945));
#17610=CARTESIAN_POINT('Ctrl Pts',(93.5135729192634,1.80451957298273,1.26565637216092));
#17611=CARTESIAN_POINT('Ctrl Pts',(93.5148187006686,1.79081440203544,1.28497501006123));
#17612=CARTESIAN_POINT('Ctrl Pts',(93.5215782978389,1.71408467482188,1.38951958398089));
#17613=CARTESIAN_POINT('Ctrl Pts',(93.5268610462018,1.64528390915837,1.4703384500147));
#17614=CARTESIAN_POINT('Ctrl Pts',(93.5383109204126,1.48084106912022,1.63744364233642));
#17615=CARTESIAN_POINT('Ctrl Pts',(93.5444037702861,1.38292960214896,1.72093443910016));
#17616=CARTESIAN_POINT('Ctrl Pts',(93.5540332142203,1.22450366422254,1.83373103132184));
#17617=CARTESIAN_POINT('Ctrl Pts',(93.5573723364798,1.16900667281692,1.86959906744733));
#17618=CARTESIAN_POINT('Ctrl Pts',(93.5616114805313,1.0995965095452,1.91015955004592));
#17619=CARTESIAN_POINT('Ctrl Pts',(93.5623749680103,1.08713466303404,1.91727937277578));
#17620=CARTESIAN_POINT('Ctrl Pts',(93.5635883638492,1.06741344226693,1.92829260781846));
#17621=CARTESIAN_POINT('Ctrl Pts',(93.5640332583898,1.06020004895935,1.93226801707187));
#17622=CARTESIAN_POINT('Ctrl Pts',(93.56487271353,1.04662704714868,1.93964941896304));
#17623=CARTESIAN_POINT('Ctrl Pts',(93.5652666847544,1.04027280106005,1.94306472830336));
#17624=CARTESIAN_POINT('Ctrl Pts',(93.5661973592173,1.02529740986403,1.95101925911956));
#17625=CARTESIAN_POINT('Ctrl Pts',(93.5667356392425,1.01666279892074,1.95553258067734));
#17626=CARTESIAN_POINT('Ctrl Pts',(93.5685297296344,0.987960169659007,1.97029400131007));
#17627=CARTESIAN_POINT('Ctrl Pts',(93.5697996930901,0.967765536414832,1.98029127516887));
#17628=CARTESIAN_POINT('Ctrl Pts',(93.5729295068077,0.918188893694589,2.00389456696331));
#17629=CARTESIAN_POINT('Ctrl Pts',(93.5748042468324,0.888653890759159,2.01716592224458));
#17630=CARTESIAN_POINT('Ctrl Pts',(93.5827219774557,0.764092711731034,2.06987010113438));
#17631=CARTESIAN_POINT('Ctrl Pts',(93.5889356350719,0.666659361619681,2.1032745706533));
#17632=CARTESIAN_POINT('Ctrl Pts',(93.6037015921959,0.428849775582664,2.16661446511029));
#17633=CARTESIAN_POINT('Ctrl Pts',(93.6121620417927,0.287164686339577,2.18990365014303));
#17634=CARTESIAN_POINT('Ctrl Pts',(93.6216975236506,0.117309340500798,2.20104088207681));
#17635=CARTESIAN_POINT('Ctrl Pts',(93.6231923520175,0.0903835592114097,
2.20231091106627));
#17636=CARTESIAN_POINT('Ctrl Pts',(93.6253105964606,0.0518079052208622,
2.20342174076335));
#17637=CARTESIAN_POINT('Ctrl Pts',(93.6259464657204,0.0401728052261094,
2.20366457968713));
#17638=CARTESIAN_POINT('Ctrl Pts',(93.6270939537324,0.0190777760891422,
2.20393772929777));
#17639=CARTESIAN_POINT('Ctrl Pts',(93.6276065381154,0.00961859671807106,
2.20399931092351));
#17640=CARTESIAN_POINT('Ctrl Pts',(93.628117219095,0.000159212296038848,
2.20399999424942));
#17641=CARTESIAN_POINT('Ctrl Pts',(93.6281172207996,0.000159180721964109,
2.2039999942517));
#17642=CARTESIAN_POINT('Ctrl Pts',(93.628120085347,0.000106120480998003,
2.2039999980839));
#17643=CARTESIAN_POINT('Ctrl Pts',(93.6281229498343,5.3060240237878E-5,
2.204));
#17644=CARTESIAN_POINT('Ctrl Pts',(93.6281258142613,-2.08913978507926E-13,
2.204));
#17645=CARTESIAN_POINT('Origin',(66.9212607628943,0.,0.));
#17646=CARTESIAN_POINT('',(94.4842111356677,-1.34689240618509E-10,2.204));
#17647=CARTESIAN_POINT('',(94.3756281550323,1.12638885946569E-10,2.204));
#17648=CARTESIAN_POINT('',(66.9212607628943,-2.69912154532077E-16,2.204));
#17649=CARTESIAN_POINT('Ctrl Pts',(94.4842111356677,-1.34689273623145E-10,
2.204));
#17650=CARTESIAN_POINT('Ctrl Pts',(94.4755329260027,0.144554936193152,2.20400000000883));
#17651=CARTESIAN_POINT('Ctrl Pts',(94.4669715239421,0.288779928745478,2.18977863375921));
#17652=CARTESIAN_POINT('Ctrl Pts',(94.4571165643329,0.460855615512199,2.15550003951819));
#17653=CARTESIAN_POINT('Ctrl Pts',(94.4554028323884,0.490991655142827,2.14883588239167));
#17654=CARTESIAN_POINT('Ctrl Pts',(94.4528430644687,0.536314841135943,2.13780997761415));
#17655=CARTESIAN_POINT('Ctrl Pts',(94.451982241008,0.551610507374334,2.13391447242889));
#17656=CARTESIAN_POINT('Ctrl Pts',(94.4504433200519,0.579047215088749,2.12661216165422));
#17657=CARTESIAN_POINT('Ctrl Pts',(94.4497633335038,0.591203255217717,2.12326486421961));
#17658=CARTESIAN_POINT('Ctrl Pts',(94.4483161854108,0.617140001045622,2.11588288471663));
#17659=CARTESIAN_POINT('Ctrl Pts',(94.4475500597095,0.63091139614224,2.11181746045393));
#17660=CARTESIAN_POINT('Ctrl Pts',(94.4454671786757,0.668452680218493,2.10033496996597));
#17661=CARTESIAN_POINT('Ctrl Pts',(94.4441592322409,0.692138527511339,2.09264910981138));
#17662=CARTESIAN_POINT('Ctrl Pts',(94.4412780147371,0.74451002619487,2.07466848902778));
#17663=CARTESIAN_POINT('Ctrl Pts',(94.4397111962772,0.773122826556533,2.06417676647542));
#17664=CARTESIAN_POINT('Ctrl Pts',(94.4347790450191,0.86342836540625,2.02892229545274));
#17665=CARTESIAN_POINT('Ctrl Pts',(94.4314792240034,0.924224275939539,2.00196016740092));
#17666=CARTESIAN_POINT('Ctrl Pts',(94.4218340523172,1.10048438414319,1.91404760938981));
#17667=CARTESIAN_POINT('Ctrl Pts',(94.4156477294851,1.21184926726234,1.8455523486277));
#17668=CARTESIAN_POINT('Ctrl Pts',(94.4057300303503,1.37297071605369,1.72555083613591));
#17669=CARTESIAN_POINT('Ctrl Pts',(94.4021815416241,1.42739088819563,1.68081165490115));
#17670=CARTESIAN_POINT('Ctrl Pts',(94.3977051666337,1.49033571375073,1.62379997956445));
#17671=CARTESIAN_POINT('Ctrl Pts',(94.396932858669,1.50100277890876,1.61394471674125));
#17672=CARTESIAN_POINT('Ctrl Pts',(94.3957111442336,1.51755768450098,1.59834362243017));
#17673=CARTESIAN_POINT('Ctrl Pts',(94.3952669307489,1.52351225618735,1.59266884879891));
#17674=CARTESIAN_POINT('Ctrl Pts',(94.3944719643773,1.53404996823727,1.58251312091587));
#17675=CARTESIAN_POINT('Ctrl Pts',(94.3941222185961,1.53864551403849,1.57804532941381));
#17676=CARTESIAN_POINT('Ctrl Pts',(94.3932727922954,1.54970983096841,1.5671943176669));
#17677=CARTESIAN_POINT('Ctrl Pts',(94.3927715743218,1.55615863396331,1.56079111013264));
#17678=CARTESIAN_POINT('Ctrl Pts',(94.3912023629604,1.57610854780816,1.54073570346931));
#17679=CARTESIAN_POINT('Ctrl Pts',(94.390124422563,1.58947063855862,1.52694718326401));
#17680=CARTESIAN_POINT('Ctrl Pts',(94.3844920145473,1.65764656257154,1.45473095159012));
#17681=CARTESIAN_POINT('Ctrl Pts',(94.3797641813018,1.70942119610173,1.39352478497471));
#17682=CARTESIAN_POINT('Ctrl Pts',(94.3665400319105,1.84297096431901,1.21697623227737));
#17683=CARTESIAN_POINT('Ctrl Pts',(94.3579739670952,1.91717512910132,1.09636596904523));
#17684=CARTESIAN_POINT('Ctrl Pts',(94.3454116421316,2.01193566200479,0.902899355661724));
#17685=CARTESIAN_POINT('Ctrl Pts',(94.3411803758647,2.04116884521913,0.834711854907595));
#17686=CARTESIAN_POINT('Ctrl Pts',(94.3358287098301,2.07463527678722,0.744311355294609));
#17687=CARTESIAN_POINT('Ctrl Pts',(94.3346040500425,2.08204272016849,0.723331934852169));
#17688=CARTESIAN_POINT('Ctrl Pts',(94.3326373353251,2.09352514243281,0.68917242601368));
#17689=CARTESIAN_POINT('Ctrl Pts',(94.331888854483,2.09779613561352,0.676060308202038));
#17690=CARTESIAN_POINT('Ctrl Pts',(94.3304571493909,2.10577302615682,0.650767270620612));
#17691=CARTESIAN_POINT('Ctrl Pts',(94.32977335555,2.10949697712415,0.638592664478323));
#17692=CARTESIAN_POINT('Ctrl Pts',(94.3281935396298,2.11789860509736,0.610249757478722));
#17693=CARTESIAN_POINT('Ctrl Pts',(94.3273001295572,2.12249701669685,0.594058669898781));
#17694=CARTESIAN_POINT('Ctrl Pts',(94.324426998515,2.13678082956936,0.541480740360065));
#17695=CARTESIAN_POINT('Ctrl Pts',(94.3224712676927,2.14571966857923,0.504897046662249));
#17696=CARTESIAN_POINT('Ctrl Pts',(94.3141972667103,2.18001368033813,0.347111368708467));
#17697=CARTESIAN_POINT('Ctrl Pts',(94.30816679732,2.19606968884809,0.224114518980948));
#17698=CARTESIAN_POINT('Ctrl Pts',(94.2951091691506,2.20837133692535,-0.0456128568451124));
#17699=CARTESIAN_POINT('Ctrl Pts',(94.2881297916571,2.20048622062959,-0.191923968391015));
#17700=CARTESIAN_POINT('Ctrl Pts',(94.2795866877272,2.17552760641784,-0.353550998567542));
#17701=CARTESIAN_POINT('Ctrl Pts',(94.278668668687,2.17266911864438,-0.370712205575144));
#17702=CARTESIAN_POINT('Ctrl Pts',(94.2772678624662,2.16805128817065,-0.396544900281867));
#17703=CARTESIAN_POINT('Ctrl Pts',(94.27679295198,2.16644233509168,-0.405242951132153));
#17704=CARTESIAN_POINT('Ctrl Pts',(94.2759257322284,2.16342728137486,-0.421011116281111));
#17705=CARTESIAN_POINT('Ctrl Pts',(94.2755344010851,2.16203875327917,-0.42808455960588));
#17706=CARTESIAN_POINT('Ctrl Pts',(94.2747185829523,2.15908705485425,-0.442740356607223));
#17707=CARTESIAN_POINT('Ctrl Pts',(94.2742938197746,2.15751860642754,-0.450321432894227));
#17708=CARTESIAN_POINT('Ctrl Pts',(94.2731666355447,2.15327235524986,-0.470314132517021));
#17709=CARTESIAN_POINT('Ctrl Pts',(94.2724605589959,2.15052721935581,-0.482710971779726));
#17710=CARTESIAN_POINT('Ctrl Pts',(94.2690893050089,2.13701072239248,-0.54134566475598));
#17711=CARTESIAN_POINT('Ctrl Pts',(94.2663567207286,2.1248549478544,-0.587248480012665));
#17712=CARTESIAN_POINT('Ctrl Pts',(94.2576956166837,2.08235623116248,-0.729056106455512));
#17713=CARTESIAN_POINT('Ctrl Pts',(94.251626214002,2.0469259610892,-0.823300103081853));
#17714=CARTESIAN_POINT('Ctrl Pts',(94.2370259418136,1.94596461217234,-1.04460323400846));
#17715=CARTESIAN_POINT('Ctrl Pts',(94.2285813858493,1.87426989969075,-1.1683738141596));
#17716=CARTESIAN_POINT('Ctrl Pts',(94.2188278364962,1.77308359070473,-1.30948332158075));
#17717=CARTESIAN_POINT('Ctrl Pts',(94.2171107187019,1.7545385013355,-1.33422890593055));
#17718=CARTESIAN_POINT('Ctrl Pts',(94.2145469469628,1.72574166342128,-1.37101466296442));
#17719=CARTESIAN_POINT('Ctrl Pts',(94.213685436762,1.71587155267967,-1.3833475080242));
#17720=CARTESIAN_POINT('Ctrl Pts',(94.212145768402,1.6978854444494,-1.4053327032635));
#17721=CARTESIAN_POINT('Ctrl Pts',(94.2114657135551,1.68981764606795,-1.41502343499562));
#17722=CARTESIAN_POINT('Ctrl Pts',(94.2100189252977,1.67239121909451,-1.43559379237224));
#17723=CARTESIAN_POINT('Ctrl Pts',(94.2092532221364,1.66300857003547,-1.44645236205736));
#17724=CARTESIAN_POINT('Ctrl Pts',(94.2071727768072,1.63708331464815,-1.47587000419676));
#17725=CARTESIAN_POINT('Ctrl Pts',(94.2058668079152,1.62033143840077,-1.49424233112496));
#17726=CARTESIAN_POINT('Ctrl Pts',(94.1965103074908,1.4969528290348,-1.6250403293642));
#17727=CARTESIAN_POINT('Ctrl Pts',(94.1889918462647,1.37904397359871,-1.7262293223493));
#17728=CARTESIAN_POINT('Ctrl Pts',(94.1750114835914,1.14093667234046,-1.89048031328777));
#17729=CARTESIAN_POINT('Ctrl Pts',(94.1685564835556,1.02366148421603,-1.95646657076188));
#17730=CARTESIAN_POINT('Ctrl Pts',(94.1605019136442,0.882728565424131,-2.01960707890652));
#17731=CARTESIAN_POINT('Ctrl Pts',(94.1594381506976,0.864217924280999,-2.02759704972671));
#17732=CARTESIAN_POINT('Ctrl Pts',(94.1578696584096,0.837134162115,-2.03884929666943));
#17733=CARTESIAN_POINT('Ctrl Pts',(94.1573763634874,0.828645671476639,-2.04231398296313));
#17734=CARTESIAN_POINT('Ctrl Pts',(94.1564951204699,0.813540513966217,-2.04836967452848));
#17735=CARTESIAN_POINT('Ctrl Pts',(94.1561084362098,0.806932592824048,-2.0509817845527));
#17736=CARTESIAN_POINT('Ctrl Pts',(94.1552634469718,0.792538271984392,-2.05659152388252));
#17737=CARTESIAN_POINT('Ctrl Pts',(94.1548044663219,0.784747560890426,-2.05957686665034));
#17738=CARTESIAN_POINT('Ctrl Pts',(94.1534869599285,0.762457040568895,-2.06797359482819));
#17739=CARTESIAN_POINT('Ctrl Pts',(94.1526224124811,0.747917208585949,-2.07327647676347));
#17740=CARTESIAN_POINT('Ctrl Pts',(94.1451748638944,0.623278475895987,-2.11725229583426));
#17741=CARTESIAN_POINT('Ctrl Pts',(94.1381936957908,0.51033363417477,-2.14727454984663));
#17742=CARTESIAN_POINT('Ctrl Pts',(94.1208700013375,0.226583140071448,-2.19904026816622));
#17743=CARTESIAN_POINT('Ctrl Pts',(94.1105980807696,0.0545569434765714,
-2.2100135847477));
#17744=CARTESIAN_POINT('Ctrl Pts',(94.0994680885465,-0.143690417938653,
-2.19947325445585));
#17745=CARTESIAN_POINT('Ctrl Pts',(94.0979852556208,-0.170337573629096,
-2.19757018833114));
#17746=CARTESIAN_POINT('Ctrl Pts',(94.0956298748282,-0.213034159776627,
-2.19373959500773));
#17747=CARTESIAN_POINT('Ctrl Pts',(94.0947478421117,-0.229107847546192,
-2.19211919788558));
#17748=CARTESIAN_POINT('Ctrl Pts',(94.0931836076428,-0.257760232961659,
-2.18891213882756));
#17749=CARTESIAN_POINT('Ctrl Pts',(94.0924993021811,-0.270345668103714,
-2.18739340730363));
#17750=CARTESIAN_POINT('Ctrl Pts',(94.0910674996146,-0.296781812468318,
-2.18397161055297));
#17751=CARTESIAN_POINT('Ctrl Pts',(94.0903207727717,-0.310628960843505,
-2.18204516473301));
#17752=CARTESIAN_POINT('Ctrl Pts',(94.0883493310487,-0.347337580166986,
-2.17658165942564));
#17753=CARTESIAN_POINT('Ctrl Pts',(94.0871318588954,-0.370163602299328,
-2.17281616245498));
#17754=CARTESIAN_POINT('Ctrl Pts',(94.0807996096661,-0.489606745909725,
-2.1511752827106));
#17755=CARTESIAN_POINT('Ctrl Pts',(94.0758811870315,-0.585012139986624,
-2.12721261051288));
#17756=CARTESIAN_POINT('Ctrl Pts',(94.0667462217839,-0.762351478572828,
-2.0698313738539));
#17757=CARTESIAN_POINT('Ctrl Pts',(94.0625163776412,-0.844493294563531,
-2.0376979614208));
#17758=CARTESIAN_POINT('Ctrl Pts',(94.0570318346265,-0.947217573138083,
-1.99023156558713));
#17759=CARTESIAN_POINT('Ctrl Pts',(94.0558152035112,-0.969764045397713,
-1.97934344848997));
#17760=CARTESIAN_POINT('Ctrl Pts',(94.0502530192008,-1.07140222953487,-1.92810692029083));
#17761=CARTESIAN_POINT('Ctrl Pts',(94.045835841344,-1.1481896513284,-1.88338961717163));
#17762=CARTESIAN_POINT('Ctrl Pts',(94.0403703586209,-1.23457791592129,-1.82583118452948));
#17763=CARTESIAN_POINT('Ctrl Pts',(94.0395713373945,-1.2470066320971,-1.81736528516943));
#17764=CARTESIAN_POINT('Ctrl Pts',(94.0383164186815,-1.26619272147761,-1.80400708573333));
#17765=CARTESIAN_POINT('Ctrl Pts',(94.0378661815826,-1.27301081731342,-1.79920233094015));
#17766=CARTESIAN_POINT('Ctrl Pts',(94.0370274410703,-1.28558669705435,-1.79023276165223));
#17767=CARTESIAN_POINT('Ctrl Pts',(94.0366396523033,-1.2913518005242,-1.78607867107639));
#17768=CARTESIAN_POINT('Ctrl Pts',(94.0357383987963,-1.30463786954054,-1.77640733861523));
#17769=CARTESIAN_POINT('Ctrl Pts',(94.035223595197,-1.31214397914477,-1.7708701744779));
#17770=CARTESIAN_POINT('Ctrl Pts',(94.0335679341264,-1.33602965786903,-1.75301476959742));
#17771=CARTESIAN_POINT('Ctrl Pts',(94.0324155622602,-1.35227219561552,-1.74051597998687));
#17772=CARTESIAN_POINT('Ctrl Pts',(94.0260068648147,-1.44067935144202,-1.67050132838555));
#17773=CARTESIAN_POINT('Ctrl Pts',(94.0205245701103,-1.50934601792695,-1.60872728705917));
#17774=CARTESIAN_POINT('Ctrl Pts',(94.0050296166324,-1.6903091583838,-1.4241169313775));
#17775=CARTESIAN_POINT('Ctrl Pts',(93.995001060159,-1.79289649630129,-1.29259063495724));
#17776=CARTESIAN_POINT('Ctrl Pts',(93.9830493245384,-1.90250050849489,-1.11355792286878));
#17777=CARTESIAN_POINT('Ctrl Pts',(93.9806026812108,-1.92417120065752,-1.07567885658972));
#17778=CARTESIAN_POINT('Ctrl Pts',(93.9771877153821,-1.9533065421853,-1.02105029295934));
#17779=CARTESIAN_POINT('Ctrl Pts',(93.9761865451057,-1.96170797451672,-1.00481441055363));
#17780=CARTESIAN_POINT('Ctrl Pts',(93.9744939846191,-1.97566747718466,-0.976994888475123));
#17781=CARTESIAN_POINT('Ctrl Pts',(93.9737990304719,-1.98132793429741,-0.965463939806464));
#17782=CARTESIAN_POINT('Ctrl Pts',(93.9723929637161,-1.99263299206583,-0.941916132673545));
#17783=CARTESIAN_POINT('Ctrl Pts',(93.9716821193975,-1.99827047187394,-0.929896431822365));
#17784=CARTESIAN_POINT('Ctrl Pts',(93.9699196131322,-2.01205017881955,-0.899812566318307));
#17785=CARTESIAN_POINT('Ctrl Pts',(93.968872583281,-2.02005814990925,-0.881687972976864));
#17786=CARTESIAN_POINT('Ctrl Pts',(93.9647637098073,-2.05075498347698,-0.809596780055301));
#17787=CARTESIAN_POINT('Ctrl Pts',(93.9617659996779,-2.07153525340022,-0.754841302692485));
#17788=CARTESIAN_POINT('Ctrl Pts',(93.9537973566608,-2.12183968627772,-0.604492560710857));
#17789=CARTESIAN_POINT('Ctrl Pts',(93.9489459130672,-2.14707856300133,-0.507612151778338));
#17790=CARTESIAN_POINT('Ctrl Pts',(93.9372734857204,-2.19192285542642,-0.270364889169396));
#17791=CARTESIAN_POINT('Ctrl Pts',(93.9305019197053,-2.20475028511078,-0.129189505346149));
#17792=CARTESIAN_POINT('Ctrl Pts',(93.9220958357517,-2.20385744177126,0.0318187137023454));
#17793=CARTESIAN_POINT('Ctrl Pts',(93.9210610612339,-2.20348740256429,0.0514127281607357));
#17794=CARTESIAN_POINT('Ctrl Pts',(93.9195224612757,-2.20256099543877,0.0801561656346075));
#17795=CARTESIAN_POINT('Ctrl Pts',(93.9190293005446,-2.20220874609843,0.0893117129892938));
#17796=CARTESIAN_POINT('Ctrl Pts',(93.9181487575143,-2.20148256736756,0.10555003003969));
#17797=CARTESIAN_POINT('Ctrl Pts',(93.9177626423583,-2.2011315235986,0.112633552907477));
#17798=CARTESIAN_POINT('Ctrl Pts',(93.9169116901552,-2.20028677740135,0.128162645728139));
#17799=CARTESIAN_POINT('Ctrl Pts',(93.9164460956575,-2.19977864548602,0.13660700033643));
#17800=CARTESIAN_POINT('Ctrl Pts',(93.9150906546537,-2.19816670936478,0.161047209297219));
#17801=CARTESIAN_POINT('Ctrl Pts',(93.9141942543842,-2.1969369720768,0.177033883603621));
#17802=CARTESIAN_POINT('Ctrl Pts',(93.9065278162353,-2.18503506853992,0.312424107077827));
#17803=CARTESIAN_POINT('Ctrl Pts',(93.8993424422437,-2.16481246936675,0.430777211013497));
#17804=CARTESIAN_POINT('Ctrl Pts',(93.8821181903364,-2.09366793878611,0.708528611365436));
#17805=CARTESIAN_POINT('Ctrl Pts',(93.8721557373993,-2.03403508891293,0.864971937865329));
#17806=CARTESIAN_POINT('Ctrl Pts',(93.8612708318752,-1.94482962318424,1.03729944259209));
#17807=CARTESIAN_POINT('Ctrl Pts',(93.8597637957971,-1.93191026705024,1.06116690934273));
#17808=CARTESIAN_POINT('Ctrl Pts',(93.8573778216672,-1.91054254792675,1.09895771096546));
#17809=CARTESIAN_POINT('Ctrl Pts',(93.85648900359,-1.90237527029695,1.11303604117105));
#17810=CARTESIAN_POINT('Ctrl Pts',(93.8549170723783,-1.88756231723248,1.13793040065963));
#17811=CARTESIAN_POINT('Ctrl Pts',(93.8542317812317,-1.88097779958548,1.14878180045678));
#17812=CARTESIAN_POINT('Ctrl Pts',(93.8528022295888,-1.86697741924999,1.17141154876758));
#17813=CARTESIAN_POINT('Ctrl Pts',(93.8520586935166,-1.85954297108029,1.18317777677668));
#17814=CARTESIAN_POINT('Ctrl Pts',(93.8501055568538,-1.83961363650393,1.21406731677005));
#17815=CARTESIAN_POINT('Ctrl Pts',(93.8489029538784,-1.8269318850441,1.23306841671087));
#17816=CARTESIAN_POINT('Ctrl Pts',(93.8428381209405,-1.76092389569107,1.32871388365581));
#17817=CARTESIAN_POINT('Ctrl Pts',(93.8381517794172,-1.70305908108346,1.40211477030022));
#17818=CARTESIAN_POINT('Ctrl Pts',(93.829079686912,-1.57975744356482,1.53958271077273));
#17819=CARTESIAN_POINT('Ctrl Pts',(93.8246976335095,-1.51464367833092,1.60368430573631));
#17820=CARTESIAN_POINT('Ctrl Pts',(93.8186737245841,-1.42078638182128,1.68525229344282));
#17821=CARTESIAN_POINT('Ctrl Pts',(93.8170669901237,-1.39534526113366,1.70637650515202));
#17822=CARTESIAN_POINT('Ctrl Pts',(93.8113662518331,-1.30418404530579,1.77866689177433));
#17823=CARTESIAN_POINT('Ctrl Pts',(93.8072070502701,-1.23605445340312,1.826668739746));
#17824=CARTESIAN_POINT('Ctrl Pts',(93.8020371332055,-1.15273581872842,1.87857341028165));
#17825=CARTESIAN_POINT('Ctrl Pts',(93.8012454167395,-1.14001230350998,1.88632177781117));
#17826=CARTESIAN_POINT('Ctrl Pts',(93.7999995738072,-1.12007095322274,1.89819021951072));
#17827=CARTESIAN_POINT('Ctrl Pts',(93.7995509781694,-1.11290647974577,1.90239959326288));
#17828=CARTESIAN_POINT('Ctrl Pts',(93.7987172854616,-1.09962598297259,1.91010164675259));
#17829=CARTESIAN_POINT('Ctrl Pts',(93.798332917789,-1.09351682331345,1.91360564275796));
#17830=CARTESIAN_POINT('Ctrl Pts',(93.7974347477554,-1.07927193067843,1.92168551721675));
#17831=CARTESIAN_POINT('Ctrl Pts',(93.7969195672158,-1.07112383915196,1.92623904076157));
#17832=CARTESIAN_POINT('Ctrl Pts',(93.7952614640521,-1.04496148098274,1.94064242885874));
#17833=CARTESIAN_POINT('Ctrl Pts',(93.7941069810965,-1.02683890501674,1.95029211523496));
#17834=CARTESIAN_POINT('Ctrl Pts',(93.7876751291781,-0.926209605777247,
2.00208262787474));
#17835=CARTESIAN_POINT('Ctrl Pts',(93.782170127685,-0.841249558976145,2.03923893800935));
#17836=CARTESIAN_POINT('Ctrl Pts',(93.7702655775841,-0.654643359567615,
2.10719883952728));
#17837=CARTESIAN_POINT('Ctrl Pts',(93.7638698039526,-0.55258383915252,2.13623451614533));
#17838=CARTESIAN_POINT('Ctrl Pts',(93.754913509879,-0.403762671966871,2.16718955117525));
#17839=CARTESIAN_POINT('Ctrl Pts',(93.7522306450708,-0.358411929414702,
2.17514967342432));
#17840=CARTESIAN_POINT('Ctrl Pts',(93.7464887600969,-0.259476925040162,
2.18933648342462));
#17841=CARTESIAN_POINT('Ctrl Pts',(93.7434460627509,-0.205845036979493,
2.19502871044619));
#17842=CARTESIAN_POINT('Ctrl Pts',(93.7393913588451,-0.132702182608141,
2.20008691841751));
#17843=CARTESIAN_POINT('Ctrl Pts',(93.7383265074971,-0.113332247361482,
2.20116972393609));
#17844=CARTESIAN_POINT('Ctrl Pts',(93.7365429726326,-0.080623317050864,
2.20256527870119));
#17845=CARTESIAN_POINT('Ctrl Pts',(93.7358201104746,-0.0672914576818401,
2.2030128907681));
#17846=CARTESIAN_POINT('Ctrl Pts',(93.7346098872167,-0.0448480070696404,
2.20356249382968));
#17847=CARTESIAN_POINT('Ctrl Pts',(93.7341205212728,-0.035738479639022,
2.20372906058751));
#17848=CARTESIAN_POINT('Ctrl Pts',(93.7331578692262,-0.0177525462416429,
2.20394637724993));
#17849=CARTESIAN_POINT('Ctrl Pts',(93.7326845030318,-0.00887635722052226,
2.204));
#17850=CARTESIAN_POINT('Ctrl Pts',(93.7322127872898,-1.52555169845894E-15,
2.204));
#17851=CARTESIAN_POINT('Ctrl Pts',(93.6281258142613,-2.08913978507926E-13,
2.204));
#17852=CARTESIAN_POINT('Ctrl Pts',(93.6287336333723,-0.0112591551814979,
2.204));
#17853=CARTESIAN_POINT('Ctrl Pts',(93.6293387394407,-0.022518296427486,
2.2039137237877));
#17854=CARTESIAN_POINT('Ctrl Pts',(93.6307286024886,-0.0484919604802062,
2.20351562898419));
#17855=CARTESIAN_POINT('Ctrl Pts',(93.6315114239032,-0.0632050857157136,
2.20314269369862));
#17856=CARTESIAN_POINT('Ctrl Pts',(93.6338368903869,-0.10715072333209,2.20158819953408));
#17857=CARTESIAN_POINT('Ctrl Pts',(93.6353659969666,-0.136365169972084,
2.19997193701538));
#17858=CARTESIAN_POINT('Ctrl Pts',(93.6473048774245,-0.366641036528467,
2.18262720805577));
#17859=CARTESIAN_POINT('Ctrl Pts',(93.6567740931849,-0.564697751164643,
2.13995414131552));
#17860=CARTESIAN_POINT('Ctrl Pts',(93.6695478127351,-0.810120517242369,
2.0505763457388));
#17861=CARTESIAN_POINT('Ctrl Pts',(93.6724963725378,-0.865196118094291,
2.02795303212838));
#17862=CARTESIAN_POINT('Ctrl Pts',(93.677303019617,-0.950744061277059,1.98869299048612));
#17863=CARTESIAN_POINT('Ctrl Pts',(93.6791006146663,-0.981856627121886,
1.97351751654895));
#17864=CARTESIAN_POINT('Ctrl Pts',(93.6815487943064,-1.02278999316325,1.952344313673));
#17865=CARTESIAN_POINT('Ctrl Pts',(93.6821628776929,-1.03294118527824,1.94699260027798));
#17866=CARTESIAN_POINT('Ctrl Pts',(93.6831877388142,-1.0496792338797,1.93800055154315));
#17867=CARTESIAN_POINT('Ctrl Pts',(93.6835957364622,-1.05629019837473,1.93440524340744));
#17868=CARTESIAN_POINT('Ctrl Pts',(93.6843710598922,-1.06875051628291,1.92754590138267));
#17869=CARTESIAN_POINT('Ctrl Pts',(93.6847379200292,-1.0746036592805,1.92428891826811));
#17870=CARTESIAN_POINT('Ctrl Pts',(93.6856151887193,-1.08850174694825,1.91647213909086));
#17871=CARTESIAN_POINT('Ctrl Pts',(93.6861270850565,-1.09653295611892,1.91188832910391));
#17872=CARTESIAN_POINT('Ctrl Pts',(93.6876918582071,-1.12085471828714,1.89780303517945));
#17873=CARTESIAN_POINT('Ctrl Pts',(93.6887539027612,-1.13705198914173,1.88814310538913));
#17874=CARTESIAN_POINT('Ctrl Pts',(93.6960922217737,-1.24703069730724,1.82062433108904));
#17875=CARTESIAN_POINT('Ctrl Pts',(93.702691806428,-1.33647556786597,1.7560147363038));
#17876=CARTESIAN_POINT('Ctrl Pts',(93.7153286775383,-1.49731043394918,1.62040651052834));
#17877=CARTESIAN_POINT('Ctrl Pts',(93.7213483601906,-1.56942478570504,1.55066560497573));
#17878=CARTESIAN_POINT('Ctrl Pts',(93.7320565384587,-1.69188073640857,1.41491358622701));
#17879=CARTESIAN_POINT('Ctrl Pts',(93.7367863396081,-1.74372700621387,1.35050340671083));
#17880=CARTESIAN_POINT('Ctrl Pts',(93.7426078167322,-1.80478696895649,1.2652487889178));
#17881=CARTESIAN_POINT('Ctrl Pts',(93.743831881397,-1.81746114043506,1.24697456084284));
#17882=CARTESIAN_POINT('Ctrl Pts',(93.7458027848477,-1.83759247484038,1.21698910962731));
#17883=CARTESIAN_POINT('Ctrl Pts',(93.7465559882761,-1.84521915616819,1.20539407441314));
#17884=CARTESIAN_POINT('Ctrl Pts',(93.7480002429084,-1.8597111975657,1.1829015675901));
#17885=CARTESIAN_POINT('Ctrl Pts',(93.7486918343562,-1.86659153540862,1.17201446520428));
#17886=CARTESIAN_POINT('Ctrl Pts',(93.7502793192397,-1.88224415579107,1.14675904695954));
#17887=CARTESIAN_POINT('Ctrl Pts',(93.7511726787168,-1.89094809673794,1.13234919103025));
#17888=CARTESIAN_POINT('Ctrl Pts',(93.7540717944158,-1.91883818234023,1.08495707885936));
#17889=CARTESIAN_POINT('Ctrl Pts',(93.7560527648294,-1.93733360653031,1.05157527375701));
#17890=CARTESIAN_POINT('Ctrl Pts',(93.7668476497605,-2.03466870231767,0.86460441527319));
#17891=CARTESIAN_POINT('Ctrl Pts',(93.775041516706,-2.09611601894787,0.702650431957959));
#17892=CARTESIAN_POINT('Ctrl Pts',(93.7880163133032,-2.16093663996481,0.443692506170338));
#17893=CARTESIAN_POINT('Ctrl Pts',(93.7926595442009,-2.17793923385807,0.350838455563421));
#17894=CARTESIAN_POINT('Ctrl Pts',(93.7986546785752,-2.19136715680751,0.23655390584678));
#17895=CARTESIAN_POINT('Ctrl Pts',(93.7997501360028,-2.19349986331265,0.215884353894427));
#17896=CARTESIAN_POINT('Ctrl Pts',(93.8013651879752,-2.19617545469124,0.185791224037283));
#17897=CARTESIAN_POINT('Ctrl Pts',(93.8018726531813,-2.19695060694801,0.176388862380202));
#17898=CARTESIAN_POINT('Ctrl Pts',(93.8027722207416,-2.1982093075537,0.15982298759138));
#17899=CARTESIAN_POINT('Ctrl Pts',(93.8031629131929,-2.19871825359597,0.152661674927733));
#17900=CARTESIAN_POINT('Ctrl Pts',(93.8040165168038,-2.19974849023385,0.137089698353008));
#17901=CARTESIAN_POINT('Ctrl Pts',(93.8044801150386,-2.2002565339156,0.128678614389766));
#17902=CARTESIAN_POINT('Ctrl Pts',(93.8057870222722,-2.20154567271148,0.105088795833398));
#17903=CARTESIAN_POINT('Ctrl Pts',(93.8066359965997,-2.20221799361621,0.0899048745588194));
#17904=CARTESIAN_POINT('Ctrl Pts',(93.8126810266257,-2.20585549267657,-0.0173342323559837));
#17905=CARTESIAN_POINT('Ctrl Pts',(93.8181267267075,-2.20320440024947,-0.109481239464676));
#17906=CARTESIAN_POINT('Ctrl Pts',(93.8249102580592,-2.19285525527252,-0.222385162907419));
#17907=CARTESIAN_POINT('Ctrl Pts',(93.8261874391232,-2.19060462044845,-0.243558446293098));
#17908=CARTESIAN_POINT('Ctrl Pts',(93.8327451920336,-2.17748831968346,-0.351981421917578));
#17909=CARTESIAN_POINT('Ctrl Pts',(93.8380362644771,-2.16171506968749,-0.438560582336383));
#17910=CARTESIAN_POINT('Ctrl Pts',(93.8490398235673,-2.1174243786285,-0.619521972479176));
#17911=CARTESIAN_POINT('Ctrl Pts',(93.8547136670615,-2.08766421985139,-0.713411240246326));
#17912=CARTESIAN_POINT('Ctrl Pts',(93.8614788548914,-2.04322166096454,-0.826682129239053));
#17913=CARTESIAN_POINT('Ctrl Pts',(93.8627619781991,-2.03437444063568,-0.848220957466346));
#17914=CARTESIAN_POINT('Ctrl Pts',(93.8648037814182,-2.01962308149178,-0.882574350665131));
#17915=CARTESIAN_POINT('Ctrl Pts',(93.8655696964814,-2.01393449846335,-0.895479047573452));
#17916=CARTESIAN_POINT('Ctrl Pts',(93.8670232617706,-2.00284290995776,-0.920000206486861));
#17917=CARTESIAN_POINT('Ctrl Pts',(93.8677116233329,-1.99746173326652,-0.931625856041603));
#17918=CARTESIAN_POINT('Ctrl Pts',(93.8692711769825,-1.98497820086649,-0.957990181228405));
#17919=CARTESIAN_POINT('Ctrl Pts',(93.8701401323573,-1.97781244231909,-0.972698107199681));
#17920=CARTESIAN_POINT('Ctrl Pts',(93.8728735893441,-1.95461025346047,-1.01900456336722));
#17921=CARTESIAN_POINT('Ctrl Pts',(93.8747171890475,-1.93797487822762,-1.05029762341759));
#17922=CARTESIAN_POINT('Ctrl Pts',(93.8855563538931,-1.83445282090702,-1.23419309803679));
#17923=CARTESIAN_POINT('Ctrl Pts',(93.8938938184469,-1.73034073615046,-1.3763624272371));
#17924=CARTESIAN_POINT('Ctrl Pts',(93.9070541069621,-1.54542852665354,-1.57427418794442));
#17925=CARTESIAN_POINT('Ctrl Pts',(93.9117404827267,-1.47596349815318,-1.63957828421042));
#17926=CARTESIAN_POINT('Ctrl Pts',(93.9177885045925,-1.38639995059095,-1.71346047977437));
#17927=CARTESIAN_POINT('Ctrl Pts',(93.9188887330871,-1.37011191383643,-1.72651235727779));
#17928=CARTESIAN_POINT('Ctrl Pts',(93.9205095559644,-1.34618302383223,-1.74513512090484));
#17929=CARTESIAN_POINT('Ctrl Pts',(93.9210178990036,-1.3386873540474,-1.75089162582198));
#17930=CARTESIAN_POINT('Ctrl Pts',(93.9219149451999,-1.32548280182915,-1.7608980642651));
#17931=CARTESIAN_POINT('Ctrl Pts',(93.922302192393,-1.31979002257752,-1.76516881504841));
#17932=CARTESIAN_POINT('Ctrl Pts',(93.9231501574687,-1.30734240366863,-1.77441319855071));
#17933=CARTESIAN_POINT('Ctrl Pts',(93.9236115733144,-1.30057992844843,-1.77937579070851));
#17934=CARTESIAN_POINT('Ctrl Pts',(93.9249066083704,-1.28162432728128,-1.79312043108407));
#17935=CARTESIAN_POINT('Ctrl Pts',(93.9257457372506,-1.26936969459584,-1.80181640290108));
#17936=CARTESIAN_POINT('Ctrl Pts',(93.9313567372293,-1.18753258469663,-1.85863935991779));
#17937=CARTESIAN_POINT('Ctrl Pts',(93.936339722643,-1.11532292312177,-1.90284683080483));
#17938=CARTESIAN_POINT('Ctrl Pts',(93.9432173894367,-1.01377566049741,-1.9572460165996));
#17939=CARTESIAN_POINT('Ctrl Pts',(93.9450533276944,-0.986494221072495,
-1.9711372791156));
#17940=CARTESIAN_POINT('Ctrl Pts',(93.9523657579225,-0.876857260786852,
-2.024116269418));
#17941=CARTESIAN_POINT('Ctrl Pts',(93.9578493012834,-0.792396846609868,
-2.05864856761366));
#17942=CARTESIAN_POINT('Ctrl Pts',(93.9687685622576,-0.616896794506573,
-2.11799650474594));
#17943=CARTESIAN_POINT('Ctrl Pts',(93.974185283782,-0.525908952390281,-2.14240382860225));
#17944=CARTESIAN_POINT('Ctrl Pts',(93.9806962797359,-0.411050054205773,
-2.16545242759511));
#17945=CARTESIAN_POINT('Ctrl Pts',(93.9819650851626,-0.38840036454108,-2.16962936395374));
#17946=CARTESIAN_POINT('Ctrl Pts',(93.9839897050202,-0.351835552883299,
-2.17578148887631));
#17947=CARTESIAN_POINT('Ctrl Pts',(93.9847525397047,-0.337960179352446,
-2.17797986070288));
#17948=CARTESIAN_POINT('Ctrl Pts',(93.986203738612,-0.311379228581965,-2.18193112815227));
#17949=CARTESIAN_POINT('Ctrl Pts',(93.9868927736704,-0.298677555354851,
-2.1837060698626));
#17950=CARTESIAN_POINT('Ctrl Pts',(93.9884585665339,-0.269633472078678,
-2.18750655792812));
#17951=CARTESIAN_POINT('Ctrl Pts',(93.9893330209238,-0.253282303271566,
-2.18946003502315));
#17952=CARTESIAN_POINT('Ctrl Pts',(93.9916537746351,-0.209552615840613,
-2.19418798245453));
#17953=CARTESIAN_POINT('Ctrl Pts',(93.9930898070505,-0.182141035067087,
-2.19663331752821));
#17954=CARTESIAN_POINT('Ctrl Pts',(94.0029344693662,0.00797648378945016,
-2.21000990056251));
#17955=CARTESIAN_POINT('Ctrl Pts',(94.0107648160588,0.171409596627473,-2.20336810998709));
#17956=CARTESIAN_POINT('Ctrl Pts',(94.0245877026155,0.453859778231991,-2.16024713040359));
#17957=CARTESIAN_POINT('Ctrl Pts',(94.0305477676455,0.573324585697993,-2.13165390454477));
#17958=CARTESIAN_POINT('Ctrl Pts',(94.0378430418371,0.705201650376367,-2.08819788718577));
#17959=CARTESIAN_POINT('Ctrl Pts',(94.0387047123868,0.720570069862809,-2.08294467699216));
#17960=CARTESIAN_POINT('Ctrl Pts',(94.040034701388,0.743941466074856,-2.07466630129696));
#17961=CARTESIAN_POINT('Ctrl Pts',(94.0404961534403,0.751987525150952,-2.07176348160489));
#17962=CARTESIAN_POINT('Ctrl Pts',(94.0413492784867,0.766742012563689,-2.06634315291636));
#17963=CARTESIAN_POINT('Ctrl Pts',(94.0417401327836,0.773455299553895,-2.0638396824325));
#17964=CARTESIAN_POINT('Ctrl Pts',(94.0426404568422,0.78881407163978,-2.05802673819502));
#17965=CARTESIAN_POINT('Ctrl Pts',(94.0431511823327,0.797450980293317,-2.05469550601569));
#17966=CARTESIAN_POINT('Ctrl Pts',(94.0447645051604,0.824507919163155,-2.04406342634091));
#17967=CARTESIAN_POINT('Ctrl Pts',(94.0458777428487,0.842850147761035,-2.03656872513847));
#17968=CARTESIAN_POINT('Ctrl Pts',(94.0548525469806,0.98837693284134,-1.97480331619096));
#17969=CARTESIAN_POINT('Ctrl Pts',(94.0632251370994,1.11029020981144,-1.90892320942486));
#17970=CARTESIAN_POINT('Ctrl Pts',(94.0805647689565,1.35048371035123,-1.74829025427942));
#17971=CARTESIAN_POINT('Ctrl Pts',(94.0894594166803,1.46684413759872,-1.65187973913397));
#17972=CARTESIAN_POINT('Ctrl Pts',(94.0992736410334,1.59018483655103,-1.52629210731244));
#17973=CARTESIAN_POINT('Ctrl Pts',(94.1006701061558,1.60759173424973,-1.50794704894518));
#17974=CARTESIAN_POINT('Ctrl Pts',(94.1028476770273,1.63449857853355,-1.47859444911243));
#17975=CARTESIAN_POINT('Ctrl Pts',(94.1036378074455,1.64421153849958,-1.46778594456842));
#17976=CARTESIAN_POINT('Ctrl Pts',(94.1051118608522,1.66223382036615,-1.447327487709));
#17977=CARTESIAN_POINT('Ctrl Pts',(94.1057967983012,1.67056774053059,-1.43770009528951));
#17978=CARTESIAN_POINT('Ctrl Pts',(94.1073297269656,1.68912482913058,-1.41588360153803));
#17979=CARTESIAN_POINT('Ctrl Pts',(94.1081757492044,1.69930045788661,-1.40365488397305));
#17980=CARTESIAN_POINT('Ctrl Pts',(94.1106557845079,1.72892265395412,-1.36726166907725));
#17981=CARTESIAN_POINT('Ctrl Pts',(94.1122747777999,1.74799294552133,-1.3427951453298));
#17982=CARTESIAN_POINT('Ctrl Pts',(94.1212575445019,1.85208896335321,-1.20326617332785));
#17983=CARTESIAN_POINT('Ctrl Pts',(94.1281964835753,1.92627094073789,-1.08054061348735));
#17984=CARTESIAN_POINT('Ctrl Pts',(94.139943922966,2.03120116212142,-0.861297729753891));
#17985=CARTESIAN_POINT('Ctrl Pts',(94.1447598715132,2.06817413754088,-0.768287312700597));
#17986=CARTESIAN_POINT('Ctrl Pts',(94.1513976595986,2.10844196122829,-0.642732600990195));
#17987=CARTESIAN_POINT('Ctrl Pts',(94.1530244959375,2.11751933703716,-0.612163694157456));
#17988=CARTESIAN_POINT('Ctrl Pts',(94.1558392275181,2.1318071349637,-0.559920251272809));
#17989=CARTESIAN_POINT('Ctrl Pts',(94.1570115627271,2.13735785235526,-0.538343463206542));
#17990=CARTESIAN_POINT('Ctrl Pts',(94.1587193841732,2.14485416879634,-0.507257994039228));
#17991=CARTESIAN_POINT('Ctrl Pts',(94.1592407034452,2.1470656975113,-0.49781418358351));
#17992=CARTESIAN_POINT('Ctrl Pts',(94.1601556393773,2.15081203668273,-0.481326860457285));
#17993=CARTESIAN_POINT('Ctrl Pts',(94.1605476723756,2.1523747369622,-0.474289947609504));
#17994=CARTESIAN_POINT('Ctrl Pts',(94.1613933439577,2.15565429229551,-0.459171884046771));
#17995=CARTESIAN_POINT('Ctrl Pts',(94.1618475495867,2.15736021605881,-0.451088838901748));
#17996=CARTESIAN_POINT('Ctrl Pts',(94.1631036262067,2.16192742783788,-0.428829738088441));
#17997=CARTESIAN_POINT('Ctrl Pts',(94.1639105095529,2.1646946421005,-0.414635057934217));
#17998=CARTESIAN_POINT('Ctrl Pts',(94.1685679884974,2.17973604137456,-0.333220552503686));
#17999=CARTESIAN_POINT('Ctrl Pts',(94.172556682083,2.18901761289181,-0.265490960917877));
#18000=CARTESIAN_POINT('Ctrl Pts',(94.1844734322497,2.20701701245976,-0.0653798293045088));
#18001=CARTESIAN_POINT('Ctrl Pts',(94.1925365281866,2.20695399425554,0.0674903382250955));
#18002=CARTESIAN_POINT('Ctrl Pts',(94.2062816590316,2.18589862653696,0.29908431293463));
#18003=CARTESIAN_POINT('Ctrl Pts',(94.2120499840789,2.17008973345864,0.397893181607666));
#18004=CARTESIAN_POINT('Ctrl Pts',(94.2189080683085,2.14237349742451,0.518071411255271));
#18005=CARTESIAN_POINT('Ctrl Pts',(94.2201961472389,2.13675944818476,0.540759937165932));
#18006=CARTESIAN_POINT('Ctrl Pts',(94.2222438966813,2.12717597949967,0.577007590527999));
#18007=CARTESIAN_POINT('Ctrl Pts',(94.223010877303,2.1234353477289,0.590624876171923));
#18008=CARTESIAN_POINT('Ctrl Pts',(94.2244652758879,2.11605352943742,0.616520430960001));
#18009=CARTESIAN_POINT('Ctrl Pts',(94.2251534190728,2.11243570993544,0.628804709127454));
#18010=CARTESIAN_POINT('Ctrl Pts',(94.226710884999,2.10396296895939,0.656675184817543));
#18011=CARTESIAN_POINT('Ctrl Pts',(94.2275779934023,2.0990415063573,0.672240468187701));
#18012=CARTESIAN_POINT('Ctrl Pts',(94.2302991953238,2.08295309983159,0.721223793201713));
#18013=CARTESIAN_POINT('Ctrl Pts',(94.2321326604006,2.07115727393851,0.754430316823035));
#18014=CARTESIAN_POINT('Ctrl Pts',(94.2429753738849,1.99576192884313,0.951557843751273));
#18015=CARTESIAN_POINT('Ctrl Pts',(94.2513236441277,1.9135334541249,1.10766447716915));
#18016=CARTESIAN_POINT('Ctrl Pts',(94.2644978449376,1.75946372857195,1.33078522260906));
#18017=CARTESIAN_POINT('Ctrl Pts',(94.2691874362034,1.70027463848923,1.40561897996181));
#18018=CARTESIAN_POINT('Ctrl Pts',(94.2752394002679,1.62244897398795,1.4918817827717));
#18019=CARTESIAN_POINT('Ctrl Pts',(94.2763399829783,1.60824390305983,1.50718393459308));
#18020=CARTESIAN_POINT('Ctrl Pts',(94.2779612342288,1.58729544461619,1.52911690818725));
#18021=CARTESIAN_POINT('Ctrl Pts',(94.2784696423442,1.58072299537368,1.53591020332835));
#18022=CARTESIAN_POINT('Ctrl Pts',(94.2793667602288,1.56912568381353,1.54774391967337));
#18023=CARTESIAN_POINT('Ctrl Pts',(94.2797540132216,1.56411981085483,1.55280258514089));
#18024=CARTESIAN_POINT('Ctrl Pts',(94.2806019380651,1.55316108867777,1.56377011688736));
#18025=CARTESIAN_POINT('Ctrl Pts',(94.2810633072883,1.54719907656801,1.56966918761325));
#18026=CARTESIAN_POINT('Ctrl Pts',(94.2823580891429,1.5304645201801,1.58603910378772));
#18027=CARTESIAN_POINT('Ctrl Pts',(94.2831970081457,1.51961856951106,1.59643385837314));
#18028=CARTESIAN_POINT('Ctrl Pts',(94.288800145217,1.44708944027138,1.66453693218984));
#18029=CARTESIAN_POINT('Ctrl Pts',(94.293774811282,1.38224359951118,1.71876439983942));
#18030=CARTESIAN_POINT('Ctrl Pts',(94.3007199893729,1.28886147607454,1.78814669180442));
#18031=CARTESIAN_POINT('Ctrl Pts',(94.3026324622335,1.26286031742984,1.806603518381));
#18032=CARTESIAN_POINT('Ctrl Pts',(94.3100816727387,1.1601843201433,1.87618769637456));
#18033=CARTESIAN_POINT('Ctrl Pts',(94.3156234931547,1.08072965325937,1.92305299036714));
#18034=CARTESIAN_POINT('Ctrl Pts',(94.3264792402995,0.916373831894321,2.00658333779552));
#18035=CARTESIAN_POINT('Ctrl Pts',(94.3317821913897,0.831628499643467,2.04316300673931));
#18036=CARTESIAN_POINT('Ctrl Pts',(94.3381800540566,0.723269182191769,2.08207170247906));
#18037=CARTESIAN_POINT('Ctrl Pts',(94.3394421217506,0.701586789984342,2.08947766589662));
#18038=CARTESIAN_POINT('Ctrl Pts',(94.341458653904,0.666453631418346,2.10086938712543));
#18039=CARTESIAN_POINT('Ctrl Pts',(94.3422200383473,0.65307381631619,2.10506703641674));
#18040=CARTESIAN_POINT('Ctrl Pts',(94.3436701460033,0.627375033145629,2.11286091010195));
#18041=CARTESIAN_POINT('Ctrl Pts',(94.3443595207881,0.61506297278531,2.11647778320735));
#18042=CARTESIAN_POINT('Ctrl Pts',(94.3459283606194,0.586830930631863,2.12450425327059));
#18043=CARTESIAN_POINT('Ctrl Pts',(94.3468054897548,0.570891456146901,2.1288428379435));
#18044=CARTESIAN_POINT('Ctrl Pts',(94.34913842456,0.52809549635576,2.13997628649839));
#18045=CARTESIAN_POINT('Ctrl Pts',(94.3505837868944,0.50115675532425,2.14644481771647));
#18046=CARTESIAN_POINT('Ctrl Pts',(94.3602477325801,0.318402464875393,2.18669945921583));
#18047=CARTESIAN_POINT('Ctrl Pts',(94.3679174200527,0.159443559683195,2.20399999999185));
#18048=CARTESIAN_POINT('Ctrl Pts',(94.3756281550323,1.1263660143479E-10,
2.204));
#18049=CARTESIAN_POINT('Origin',(66.9212607628943,0.,0.));
#18050=CARTESIAN_POINT('',(95.2361698906488,-1.9935815181446E-11,2.204));
#18051=CARTESIAN_POINT('',(95.1243866264839,2.95873024051195E-11,2.204));
#18052=CARTESIAN_POINT('',(66.9212607628943,-2.69912154532077E-16,2.204));
#18053=CARTESIAN_POINT('',(95.2361199581431,0.000963537602863376,2.20400005961913));
#18054=CARTESIAN_POINT('Ctrl Pts',(95.2361698906488,-1.9935815181446E-11,
2.204));
#18055=CARTESIAN_POINT('Ctrl Pts',(95.2361534167709,0.000320954503179185,
2.204));
#18056=CARTESIAN_POINT('Ctrl Pts',(95.2361369400511,0.000641910946360297,
2.20399992989215));
#18057=CARTESIAN_POINT('Ctrl Pts',(95.2361204604807,0.000962869286795163,
2.20399978967393));
#18058=CARTESIAN_POINT('Ctrl Pts',(95.2361204249416,0.000963561450979549,
2.20399978937144));
#18059=CARTESIAN_POINT('Ctrl Pts',(95.235034291354,0.0221172408984992,2.20399054124439));
#18060=CARTESIAN_POINT('Ctrl Pts',(95.2339362974794,0.0432690499204987,
2.20367674869492));
#18061=CARTESIAN_POINT('Ctrl Pts',(95.2320670260183,0.0787998801185974,
2.20263790837682));
#18062=CARTESIAN_POINT('Ctrl Pts',(95.2313035034934,0.0931825240550623,
2.2020763320936));
#18063=CARTESIAN_POINT('Ctrl Pts',(95.2301493654033,0.114704524566008,2.20102477565529));
#18064=CARTESIAN_POINT('Ctrl Pts',(95.2297643210824,0.121848945618526,2.20064082089274));
#18065=CARTESIAN_POINT('Ctrl Pts',(95.2290094347842,0.135782261522555,2.19982395966916));
#18066=CARTESIAN_POINT('Ctrl Pts',(95.2286397739114,0.142571301378628,2.19939439381365));
#18067=CARTESIAN_POINT('Ctrl Pts',(95.2278371408031,0.157236031786589,2.19839832052389));
#18068=CARTESIAN_POINT('Ctrl Pts',(95.2274035867278,0.16511073059419,2.19782091809055));
#18069=CARTESIAN_POINT('Ctrl Pts',(95.2262281816644,0.1863403244267,2.19614954718092));
#18070=CARTESIAN_POINT('Ctrl Pts',(95.2254821220025,0.199688415309678,2.19497609750168));
#18071=CARTESIAN_POINT('Ctrl Pts',(95.2219143401863,0.262972317062414,2.18883070555597));
#18072=CARTESIAN_POINT('Ctrl Pts',(95.2190182477043,0.312736353958185,2.18227623078205));
#18073=CARTESIAN_POINT('Ctrl Pts',(95.2078279590943,0.50090670280392,2.15092392354501));
#18074=CARTESIAN_POINT('Ctrl Pts',(95.1992580400119,0.637053700804592,2.11460271663876));
#18075=CARTESIAN_POINT('Ctrl Pts',(95.1842853950377,0.873312631742267,2.0266656605574));
#18076=CARTESIAN_POINT('Ctrl Pts',(95.1778175205937,0.974718920767726,1.97989328345489));
#18077=CARTESIAN_POINT('Ctrl Pts',(95.1702883970305,1.09294492822253,1.9140672095617));
#18078=CARTESIAN_POINT('Ctrl Pts',(95.1689766546022,1.11354092839653,1.90215892140788));
#18079=CARTESIAN_POINT('Ctrl Pts',(95.166905421712,1.14604929658732,1.88265408658885));
#18080=CARTESIAN_POINT('Ctrl Pts',(95.1661382050772,1.15808799446417,1.87527267619657));
#18081=CARTESIAN_POINT('Ctrl Pts',(95.1646919929783,1.18077148234855,1.8610627645891));
#18082=CARTESIAN_POINT('Ctrl Pts',(95.1640121848691,1.19143001854378,1.85425737895985));
#18083=CARTESIAN_POINT('Ctrl Pts',(95.1624710440022,1.21557934301188,1.83854404035458));
#18084=CARTESIAN_POINT('Ctrl Pts',(95.1616119025858,1.22903195962704,1.82957858222485));
#18085=CARTESIAN_POINT('Ctrl Pts',(95.1593772704201,1.26398298200435,1.80572610132774));
#18086=CARTESIAN_POINT('Ctrl Pts',(95.1580107170575,1.28531753391579,1.79060287168786));
#18087=CARTESIAN_POINT('Ctrl Pts',(95.1474854028872,1.44912051622182,1.67005286316826));
#18088=CARTESIAN_POINT('Ctrl Pts',(95.139031833913,1.578667907882,1.54817277635287));
#18089=CARTESIAN_POINT('Ctrl Pts',(95.12498508029,1.76430809959199,1.3257037696467));
#18090=CARTESIAN_POINT('Ctrl Pts',(95.1194754492507,1.82966199575958,1.23393876170364));
#18091=CARTESIAN_POINT('Ctrl Pts',(95.1127469769345,1.89564245244932,1.12445157263748));
#18092=CARTESIAN_POINT('Ctrl Pts',(95.1119314307482,1.90342799846769,1.11122161389339));
#18093=CARTESIAN_POINT('Ctrl Pts',(95.110660901158,1.91521738037532,1.09070048692753));
#18094=CARTESIAN_POINT('Ctrl Pts',(95.1102119395426,1.91931934800904,1.08346592102867));
#18095=CARTESIAN_POINT('Ctrl Pts',(95.1093742688837,1.92685179073015,1.07000407594121));
#18096=CARTESIAN_POINT('Ctrl Pts',(95.1089862571221,1.93029319280301,1.06378321624338));
#18097=CARTESIAN_POINT('Ctrl Pts',(95.1080913765542,1.93812198763543,1.04946839923132));
#18098=CARTESIAN_POINT('Ctrl Pts',(95.1075832542255,1.94248881721917,1.04136350459573));
#18099=CARTESIAN_POINT('Ctrl Pts',(95.1059412231075,1.95635519134849,1.01523662197354));
#18100=CARTESIAN_POINT('Ctrl Pts',(95.1047958887181,1.96565542105491,0.997110695217857));
#18101=CARTESIAN_POINT('Ctrl Pts',(95.0963711596122,2.03150955616834,0.86425977290282));
#18102=CARTESIAN_POINT('Ctrl Pts',(95.0886566902527,2.07822856813308,0.744941207618189));
#18103=CARTESIAN_POINT('Ctrl Pts',(95.0744496687078,2.1450114881738,0.518022526023417));
#18104=CARTESIAN_POINT('Ctrl Pts',(95.067965488725,2.16794032957263,0.41165531179129));
#18105=CARTESIAN_POINT('Ctrl Pts',(95.0593128611373,2.18860861591518,0.263254048796924));
#18106=CARTESIAN_POINT('Ctrl Pts',(95.0569660405474,2.19314365740099,0.222332115690185));
#18107=CARTESIAN_POINT('Ctrl Pts',(95.0528875336054,2.19911568941843,0.149980388134773));
#18108=CARTESIAN_POINT('Ctrl Pts',(95.0511420358666,2.2010310004753,0.118602744839227));
#18109=CARTESIAN_POINT('Ctrl Pts',(95.0485564715739,2.2028953475529,0.0715144192108333));
#18110=CARTESIAN_POINT('Ctrl Pts',(95.0477008013508,2.20334867824945,0.0558287062442669));
#18111=CARTESIAN_POINT('Ctrl Pts',(95.0461737218198,2.20386184573531,0.0276559062943479));
#18112=CARTESIAN_POINT('Ctrl Pts',(95.0455004185594,2.20398315373905,0.0151707356315025));
#18113=CARTESIAN_POINT('Ctrl Pts',(95.0440587550774,2.20401588316389,-0.0116951525354532));
#18114=CARTESIAN_POINT('Ctrl Pts',(95.0432915092199,2.20389266473295,-0.0260753822545955));
#18115=CARTESIAN_POINT('Ctrl Pts',(95.0412362449073,2.2031816044467,-0.064808951448164));
#18116=CARTESIAN_POINT('Ctrl Pts',(95.0399564557445,2.20233073985652,-0.0891558005461899));
#18117=CARTESIAN_POINT('Ctrl Pts',(95.0315932389294,2.19405778963238,-0.249613337088624));
#18118=CARTESIAN_POINT('Ctrl Pts',(95.0249103787182,2.17442615927617,-0.384802077922835));
#18119=CARTESIAN_POINT('Ctrl Pts',(95.0130030172164,2.11669629057034,-0.623882905709597));
#18120=CARTESIAN_POINT('Ctrl Pts',(95.007758015422,2.08305285455629,-0.728369063763963));
#18121=CARTESIAN_POINT('Ctrl Pts',(95.0004310549454,2.02786269836783,-0.864149695421951));
#18122=CARTESIAN_POINT('Ctrl Pts',(94.9985573938579,2.01308827797242,-0.898029597374532));
#18123=CARTESIAN_POINT('Ctrl Pts',(94.9953613567737,1.98699335988482,-0.953985225592102));
#18124=CARTESIAN_POINT('Ctrl Pts',(94.9940607935359,1.97613909571453,-0.97627075955252));
#18125=CARTESIAN_POINT('Ctrl Pts',(94.9922023792946,1.96035647797519,-1.00733291792418));
#18126=CARTESIAN_POINT('Ctrl Pts',(94.9916624810694,1.9557399792254,-1.01626682227587));
#18127=CARTESIAN_POINT('Ctrl Pts',(94.9907294643382,1.94771303597018,-1.03154340022193));
#18128=CARTESIAN_POINT('Ctrl Pts',(94.9903381850216,1.94433229484852,-1.03790162519033));
#18129=CARTESIAN_POINT('Ctrl Pts',(94.9895111156178,1.93715754938451,-1.05123722563457));
#18130=CARTESIAN_POINT('Ctrl Pts',(94.989074936077,1.93335694718378,-1.05821074762367));
#18131=CARTESIAN_POINT('Ctrl Pts',(94.9878850716683,1.92294107939062,-1.07707884950993));
#18132=CARTESIAN_POINT('Ctrl Pts',(94.9871270062952,1.91625329581452,-1.08893274816912));
#18133=CARTESIAN_POINT('Ctrl Pts',(94.9834050139651,1.88314172091705,-1.146372330892));
#18134=CARTESIAN_POINT('Ctrl Pts',(94.9803590507822,1.85520046105624,-1.19105948231881));
#18135=CARTESIAN_POINT('Ctrl Pts',(94.9700425056672,1.75685411846685,-1.33647926243897));
#18136=CARTESIAN_POINT('Ctrl Pts',(94.9625800219913,1.67963161745368,-1.43232346963056));
#18137=CARTESIAN_POINT('Ctrl Pts',(94.9477658579539,1.50829172585012,-1.61195230976075));
#18138=CARTESIAN_POINT('Ctrl Pts',(94.9404493399489,1.4141655600777,-1.69513360243851));
#18139=CARTESIAN_POINT('Ctrl Pts',(94.9321142539047,1.29395568143355,-1.78434436404062));
#18140=CARTESIAN_POINT('Ctrl Pts',(94.9307740328803,1.27420983714685,-1.79849811582516));
#18141=CARTESIAN_POINT('Ctrl Pts',(94.9286686732144,1.24253326774592,-1.82042015417996));
#18142=CARTESIAN_POINT('Ctrl Pts',(94.9278953630936,1.23075475787889,-1.82840400309037));
#18143=CARTESIAN_POINT('Ctrl Pts',(94.9264439770461,1.20837981936524,-1.84325625942839));
#18144=CARTESIAN_POINT('Ctrl Pts',(94.9257650131254,1.1978001204572,-1.85014872548477));
#18145=CARTESIAN_POINT('Ctrl Pts',(94.9242342025997,1.17369472654239,-1.86555947889423));
#18146=CARTESIAN_POINT('Ctrl Pts',(94.9233844331037,1.16013434525974,-1.87402235834642));
#18147=CARTESIAN_POINT('Ctrl Pts',(94.9211913374608,1.12468187317863,-1.89561554201962));
#18148=CARTESIAN_POINT('Ctrl Pts',(94.9198563984633,1.10265130626867,-1.90851454435554));
#18149=CARTESIAN_POINT('Ctrl Pts',(94.9090749537497,0.921226363175545,-2.0105493212117));
#18150=CARTESIAN_POINT('Ctrl Pts',(94.9003864863108,0.751548646407268,-2.07993878901998));
#18151=CARTESIAN_POINT('Ctrl Pts',(94.8862642060755,0.470631081367228,-2.15589117266787));
#18152=CARTESIAN_POINT('Ctrl Pts',(94.8809422137238,0.364083155954069,-2.17641876824584));
#18153=CARTESIAN_POINT('Ctrl Pts',(94.874433432658,0.241279882483361,-2.19080669527446));
#18154=CARTESIAN_POINT('Ctrl Pts',(94.8736207425861,0.226070421096619,-2.19242835607495));
#18155=CARTESIAN_POINT('Ctrl Pts',(94.872353729714,0.202578854612774,-2.19468603227857));
#18156=CARTESIAN_POINT('Ctrl Pts',(94.8719053762367,0.194307682139324,-2.19543378235174));
#18157=CARTESIAN_POINT('Ctrl Pts',(94.871068210702,0.178946681053206,-2.19673499907297));
#18158=CARTESIAN_POINT('Ctrl Pts',(94.8706800876153,0.1718581742011,-2.19730092024401));
#18159=CARTESIAN_POINT('Ctrl Pts',(94.8697841413254,0.155569351669554,-2.19852206051814));
#18160=CARTESIAN_POINT('Ctrl Pts',(94.8692750536711,0.146367547925755,-2.1991538391913));
#18161=CARTESIAN_POINT('Ctrl Pts',(94.8676680549721,0.117477854212301,-2.20095523229551));
#18162=CARTESIAN_POINT('Ctrl Pts',(94.8665596339758,0.0977785833283383,
-2.20191831693362));
#18163=CARTESIAN_POINT('Ctrl Pts',(94.8577161902663,-0.0578669185339179,
-2.20743503057469));
#18164=CARTESIAN_POINT('Ctrl Pts',(94.8494870869832,-0.193948241748064,
-2.1996584259774));
#18165=CARTESIAN_POINT('Ctrl Pts',(94.8321449184953,-0.479651929512035,
-2.15660294673373));
#18166=CARTESIAN_POINT('Ctrl Pts',(94.8231113219096,-0.628109524122365,
-2.11813469312318));
#18167=CARTESIAN_POINT('Ctrl Pts',(94.8131805211587,-0.794983783736224,
-2.05578460829656));
#18168=CARTESIAN_POINT('Ctrl Pts',(94.8117905862858,-0.818410555507513,
-2.04657123231314));
#18169=CARTESIAN_POINT('Ctrl Pts',(94.8096257451738,-0.85499860784024,-2.03145297895365));
#18170=CARTESIAN_POINT('Ctrl Pts',(94.8088418661278,-0.86826802523822,-2.02581698960101));
#18171=CARTESIAN_POINT('Ctrl Pts',(94.8073810912693,-0.893031026706379,
-2.01501126026169));
#18172=CARTESIAN_POINT('Ctrl Pts',(94.8067031798594,-0.904537362872433,
-2.00987237454781));
#18173=CARTESIAN_POINT('Ctrl Pts',(94.805188253072,-0.930278418503375,-1.99811024067187));
#18174=CARTESIAN_POINT('Ctrl Pts',(94.804353136375,-0.944487792810443,-1.99143297560836));
#18175=CARTESIAN_POINT('Ctrl Pts',(94.8019131369097,-0.986046874456804,
-1.97135866241666));
#18176=CARTESIAN_POINT('Ctrl Pts',(94.8003226844289,-1.01319221663068,-1.95754567382915));
#18177=CARTESIAN_POINT('Ctrl Pts',(94.7906560052066,-1.17824084975404,-1.86920682850032));
#18178=CARTESIAN_POINT('Ctrl Pts',(94.7831046846063,-1.3081539053577,-1.78070884483692));
#18179=CARTESIAN_POINT('Ctrl Pts',(94.7692489477125,-1.5264897961657,-1.59508518032524));
#18180=CARTESIAN_POINT('Ctrl Pts',(94.7629644610338,-1.6177585434519,-1.50243703220189));
#18181=CARTESIAN_POINT('Ctrl Pts',(94.7553208821739,-1.71017706520948,-1.39037754629946));
#18182=CARTESIAN_POINT('Ctrl Pts',(94.7544991678363,-1.71989366412518,-1.37833997001578));
#18183=CARTESIAN_POINT('Ctrl Pts',(94.7532210452214,-1.73465329049182,-1.35965567199704));
#18184=CARTESIAN_POINT('Ctrl Pts',(94.7527707727349,-1.73978682458111,-1.35308070157673));
#18185=CARTESIAN_POINT('Ctrl Pts',(94.7519320023424,-1.74922405065409,-1.34085111620507));
#18186=CARTESIAN_POINT('Ctrl Pts',(94.7515442195634,-1.75353786264935,-1.33520464908103));
#18187=CARTESIAN_POINT('Ctrl Pts',(94.7506515887248,-1.76335625653888,-1.32222343418918));
#18188=CARTESIAN_POINT('Ctrl Pts',(94.7501455103028,-1.76884242930961,-1.31487510871631));
#18189=CARTESIAN_POINT('Ctrl Pts',(94.7485167790847,-1.78624953605257,-1.29125347018468));
#18190=CARTESIAN_POINT('Ctrl Pts',(94.7473829486007,-1.79799264936999,-1.27485109064596));
#18191=CARTESIAN_POINT('Ctrl Pts',(94.7386147721744,-1.88612396260674,-1.14811217772825));
#18192=CARTESIAN_POINT('Ctrl Pts',(94.7305011038329,-1.95251109037437,-1.03117447493581));
#18193=CARTESIAN_POINT('Ctrl Pts',(94.7161772305613,-2.05091244200055,-0.813805043572388));
#18194=CARTESIAN_POINT('Ctrl Pts',(94.7099584429775,-2.0871653996624,-0.715726568664627));
#18195=CARTESIAN_POINT('Ctrl Pts',(94.700467685991,-2.13310644386122,-0.557747925577904));
#18196=CARTESIAN_POINT('Ctrl Pts',(94.6970678167327,-2.14751854418209,-0.499390552193682));
#18197=CARTESIAN_POINT('Ctrl Pts',(94.6926375361158,-2.16352444776319,-0.42092472794631));
#18198=CARTESIAN_POINT('Ctrl Pts',(94.6915400276347,-2.16725354628873,-0.401282650983361));
#18199=CARTESIAN_POINT('Ctrl Pts',(94.6897258679657,-2.17301980079748,-0.368480883056216));
#18200=CARTESIAN_POINT('Ctrl Pts',(94.6890045276649,-2.17520583035337,-0.355348874123209));
#18201=CARTESIAN_POINT('Ctrl Pts',(94.687595971072,-2.17926312204301,-0.329533879403545));
#18202=CARTESIAN_POINT('Ctrl Pts',(94.6869085083772,-2.18114296809764,-0.316852797178928));
#18203=CARTESIAN_POINT('Ctrl Pts',(94.6852567345983,-2.18541516806019,-0.286191420545203));
#18204=CARTESIAN_POINT('Ctrl Pts',(94.6842959584682,-2.18769643320147,-0.268196436409533));
#18205=CARTESIAN_POINT('Ctrl Pts',(94.6811038473573,-2.19458532623544,-0.207898676397314));
#18206=CARTESIAN_POINT('Ctrl Pts',(94.6789037521193,-2.19819017653519,-0.165489784054177));
#18207=CARTESIAN_POINT('Ctrl Pts',(94.6682138190484,-2.20990147646216,0.0440323985060621));
#18208=CARTESIAN_POINT('Ctrl Pts',(94.6602776964772,-2.20019065038445,0.21158057162421));
#18209=CARTESIAN_POINT('Ctrl Pts',(94.6476357512053,-2.15579778035772,0.467687398990503));
#18210=CARTESIAN_POINT('Ctrl Pts',(94.6430693362984,-2.13424191325306,0.557856511142384));
#18211=CARTESIAN_POINT('Ctrl Pts',(94.6371721881968,-2.10106050872926,0.66601966144325));
#18212=CARTESIAN_POINT('Ctrl Pts',(94.6360895178568,-2.09476593540462,0.685560403608739));
#18213=CARTESIAN_POINT('Ctrl Pts',(94.6344928787604,-2.08521386756964,0.713853099137779));
#18214=CARTESIAN_POINT('Ctrl Pts',(94.6339907527263,-2.08217208954237,0.722677316518574));
#18215=CARTESIAN_POINT('Ctrl Pts',(94.6331039767517,-2.07673696826687,0.738125440852542));
#18216=CARTESIAN_POINT('Ctrl Pts',(94.6327207399044,-2.07436779439653,0.74475758070498));
#18217=CARTESIAN_POINT('Ctrl Pts',(94.6318811041838,-2.06913384529123,0.759190479382962));
#18218=CARTESIAN_POINT('Ctrl Pts',(94.631424015605,-2.06625677266356,0.766986309193326));
#18219=CARTESIAN_POINT('Ctrl Pts',(94.6301405320204,-2.05809859330971,0.788712963103273));
#18220=CARTESIAN_POINT('Ctrl Pts',(94.6293087134069,-2.05272031400722,0.802606532306444));
#18221=CARTESIAN_POINT('Ctrl Pts',(94.6237780017179,-2.01633326036626,0.893845649029568));
#18222=CARTESIAN_POINT('Ctrl Pts',(94.6188738690157,-1.98110259542662,0.969427575944329));
#18223=CARTESIAN_POINT('Ctrl Pts',(94.6119866657102,-1.92649429640844,1.07110508175645));
#18224=CARTESIAN_POINT('Ctrl Pts',(94.6100616094788,-1.9106906086445,1.09904855367106));
#18225=CARTESIAN_POINT('Ctrl Pts',(94.6026644779208,-1.84772537843845,1.20491581884325));
#18226=CARTESIAN_POINT('Ctrl Pts',(94.5971856007205,-1.79635878213794,1.28023735504981));
#18227=CARTESIAN_POINT('Ctrl Pts',(94.5862550313957,-1.68258466530683,1.42668474142382));
#18228=CARTESIAN_POINT('Ctrl Pts',(94.5808233012484,-1.61996119534367,1.49741437338544));
#18229=CARTESIAN_POINT('Ctrl Pts',(94.5743055809071,-1.53673671437914,1.58005723463099));
#18230=CARTESIAN_POINT('Ctrl Pts',(94.5730438219896,-1.5202334454677,1.59594201688346));
#18231=CARTESIAN_POINT('Ctrl Pts',(94.571032557923,-1.49329885332566,1.62107020312033));
#18232=CARTESIAN_POINT('Ctrl Pts',(94.570276084166,-1.48302256647159,1.63047666301964));
#18233=CARTESIAN_POINT('Ctrl Pts',(94.5688384817129,-1.46321702831027,1.64826361241219));
#18234=CARTESIAN_POINT('Ctrl Pts',(94.5681566772875,-1.45370326649285,1.65666044507058));
#18235=CARTESIAN_POINT('Ctrl Pts',(94.566609550832,-1.43184237692007,1.67562150747281));
#18236=CARTESIAN_POINT('Ctrl Pts',(94.5657464534221,-1.41944979736318,1.68613235557603));
#18237=CARTESIAN_POINT('Ctrl Pts',(94.5634614017015,-1.38612460232055,1.71376952841054));
#18238=CARTESIAN_POINT('Ctrl Pts',(94.5620493238293,-1.36499077232947,1.73064949775185));
#18239=CARTESIAN_POINT('Ctrl Pts',(94.5519606208862,-1.21026655704501,1.84963267221418));
#18240=CARTESIAN_POINT('Ctrl Pts',(94.5439059182204,-1.06569385211044,1.9365401087172));
#18241=CARTESIAN_POINT('Ctrl Pts',(94.5299652239656,-0.803561649952779,
2.05578789240313));
#18242=CARTESIAN_POINT('Ctrl Pts',(94.5241256282431,-0.690634770208763,
2.09642366112328));
#18243=CARTESIAN_POINT('Ctrl Pts',(94.5170090817207,-0.560092942335982,
2.13170113889706));
#18244=CARTESIAN_POINT('Ctrl Pts',(94.5161898261469,-0.545163222984276,
2.13556804700443));
#18245=CARTESIAN_POINT('Ctrl Pts',(94.5149147299864,-0.522107505112866,
2.14128213249482));
#18246=CARTESIAN_POINT('Ctrl Pts',(94.5144649796325,-0.514009270853523,
2.14324050976239));
#18247=CARTESIAN_POINT('Ctrl Pts',(94.5136266490381,-0.498982642042792,
2.14678430167562));
#18248=CARTESIAN_POINT('Ctrl Pts',(94.5132387768276,-0.492057460226592,
2.1483821741579));
#18249=CARTESIAN_POINT('Ctrl Pts',(94.5123452575692,-0.476165233616216,
2.15196817572778));
#18250=CARTESIAN_POINT('Ctrl Pts',(94.5118383709981,-0.4671933852342,2.15393377188569));
#18251=CARTESIAN_POINT('Ctrl Pts',(94.5102043896584,-0.438400797491839,
2.16005343885146));
#18252=CARTESIAN_POINT('Ctrl Pts',(94.5090660196636,-0.418535533573185,
2.16399031088738));
#18253=CARTESIAN_POINT('Ctrl Pts',(94.5003582155636,-0.267775662567264,
2.19171423353927));
#18254=CARTESIAN_POINT('Ctrl Pts',(94.4923181198752,-0.135031132672781,
2.20387769499502));
#18255=CARTESIAN_POINT('Ctrl Pts',(94.4842916325511,-0.00134083298710741,
2.20399969411079));
#18256=CARTESIAN_POINT('Ctrl Pts',(94.4842513832266,-0.000670412990111774,
2.20399999999996));
#18257=CARTESIAN_POINT('Ctrl Pts',(94.4842111356677,-1.34689240618509E-10,
2.204));
#18258=CARTESIAN_POINT('',(95.1243292764227,0.000992167725779152,2.20400002542528));
#18259=CARTESIAN_POINT('Ctrl Pts',(94.3756281550323,1.12638885946569E-10,
2.204));
#18260=CARTESIAN_POINT('Ctrl Pts',(94.3756603584168,-0.000665905572939986,
2.20400000000003));
#18261=CARTESIAN_POINT('Ctrl Pts',(94.3756925632963,-0.00133181967448933,
2.20399969821039));
#18262=CARTESIAN_POINT('Ctrl Pts',(94.3814370060071,-0.120107845755977,
2.2038920376001));
#18263=CARTESIAN_POINT('Ctrl Pts',(94.3871674758867,-0.238006547199598,
2.19429103065167));
#18264=CARTESIAN_POINT('Ctrl Pts',(94.3943898537762,-0.374833827996369,
2.17198936119313));
#18265=CARTESIAN_POINT('Ctrl Pts',(94.3954728914742,-0.395065404477184,
2.1684006664732));
#18266=CARTESIAN_POINT('Ctrl Pts',(94.3970750084256,-0.424509131606257,
2.16275218550346));
#18267=CARTESIAN_POINT('Ctrl Pts',(94.3975823208827,-0.43376345833301,2.16091514742445));
#18268=CARTESIAN_POINT('Ctrl Pts',(94.3984825076259,-0.450055370000045,
2.15757223671038));
#18269=CARTESIAN_POINT('Ctrl Pts',(94.3988739814633,-0.457097789643795,
2.15609123235015));
#18270=CARTESIAN_POINT('Ctrl Pts',(94.3997224283165,-0.472267062230176,
2.15282350751547));
#18271=CARTESIAN_POINT('Ctrl Pts',(94.4001800119445,-0.480390961667001,
2.15102527922317));
#18272=CARTESIAN_POINT('Ctrl Pts',(94.4014767735422,-0.503260164331028,
2.14582715759506));
#18273=CARTESIAN_POINT('Ctrl Pts',(94.4023216249636,-0.51798063809598,2.14232140817679));
#18274=CARTESIAN_POINT('Ctrl Pts',(94.408509077786,-0.624604415317,2.11576530881441));
#18275=CARTESIAN_POINT('Ctrl Pts',(94.4141170458627,-0.714964907046716,
2.08696318169097));
#18276=CARTESIAN_POINT('Ctrl Pts',(94.428827143887,-0.943795594881254,1.99741477382729));
#18277=CARTESIAN_POINT('Ctrl Pts',(94.437961870912,-1.07839850063502,1.92807712305759));
#18278=CARTESIAN_POINT('Ctrl Pts',(94.4501225136957,-1.25481204349963,1.81290416886955));
#18279=CARTESIAN_POINT('Ctrl Pts',(94.4535010828379,-1.3034228480651,1.77827574302474));
#18280=CARTESIAN_POINT('Ctrl Pts',(94.4579509887189,-1.36692043279413,1.72903802857983));
#18281=CARTESIAN_POINT('Ctrl Pts',(94.4590876281688,-1.38308986876587,1.71613123916088));
#18282=CARTESIAN_POINT('Ctrl Pts',(94.4609536206613,-1.40954468585156,1.69439763734456));
#18283=CARTESIAN_POINT('Ctrl Pts',(94.4616881254762,-1.41993441027096,1.68570040543558));
#18284=CARTESIAN_POINT('Ctrl Pts',(94.4631214951614,-1.44015962619177,1.66845021270613));
#18285=CARTESIAN_POINT('Ctrl Pts',(94.463820622714,-1.45000074061522,1.6599047332576));
#18286=CARTESIAN_POINT('Ctrl Pts',(94.465480402562,-1.47330248513692,1.63930541420828));
#18287=CARTESIAN_POINT('Ctrl Pts',(94.4664376893326,-1.48669193782314,1.62717225942816));
#18288=CARTESIAN_POINT('Ctrl Pts',(94.4697371336208,-1.53264337467385,1.58449158278119));
#18289=CARTESIAN_POINT('Ctrl Pts',(94.4720440914672,-1.56442629826278,1.5531194417556));
#18290=CARTESIAN_POINT('Ctrl Pts',(94.4776793394126,-1.64085384205909,1.47295124449219));
#18291=CARTESIAN_POINT('Ctrl Pts',(94.4809618613709,-1.68429762687299,1.42307027012563));
#18292=CARTESIAN_POINT('Ctrl Pts',(94.490380402647,-1.80395091522768,1.27251781388112));
#18293=CARTESIAN_POINT('Ctrl Pts',(94.4963708138563,-1.8738342020333,1.16716936691133));
#18294=CARTESIAN_POINT('Ctrl Pts',(94.5062557194725,-1.97007732161288,0.990947608061888));
#18295=CARTESIAN_POINT('Ctrl Pts',(94.5100033845764,-2.00248616266083,0.923703958155115));
#18296=CARTESIAN_POINT('Ctrl Pts',(94.5147125526,-2.03716335532569,0.841308871634398));
#18297=CARTESIAN_POINT('Ctrl Pts',(94.5154994511445,-2.0427681408028,0.827607064443033));
#18298=CARTESIAN_POINT('Ctrl Pts',(94.5167419694619,-2.05131328635725,0.806101312884716));
#18299=CARTESIAN_POINT('Ctrl Pts',(94.5171921723073,-2.05434820126022,0.798335135613543));
#18300=CARTESIAN_POINT('Ctrl Pts',(94.5179965230591,-2.05966021507238,0.784511108820873));
#18301=CARTESIAN_POINT('Ctrl Pts',(94.5183496238474,-2.06195479903506,0.778460201139327));
#18302=CARTESIAN_POINT('Ctrl Pts',(94.5192058439,-2.06742945941987,0.763829273339396));
#18303=CARTESIAN_POINT('Ctrl Pts',(94.5197105122668,-2.07058276322769,0.755239526897));
#18304=CARTESIAN_POINT('Ctrl Pts',(94.5212857947462,-2.08020229020692,0.728522372076816));
#18305=CARTESIAN_POINT('Ctrl Pts',(94.5223663736296,-2.0864844573493,0.710330185616078));
#18306=CARTESIAN_POINT('Ctrl Pts',(94.5279854006355,-2.11759212056749,0.616272217557925));
#18307=CARTESIAN_POINT('Ctrl Pts',(94.5326957119678,-2.13851919186233,0.539185872900125));
#18308=CARTESIAN_POINT('Ctrl Pts',(94.549582625566,-2.19766874144523,0.262741197554854));
#18309=CARTESIAN_POINT('Ctrl Pts',(94.5618807067509,-2.21252895118918,0.059380895671477));
#18310=CARTESIAN_POINT('Ctrl Pts',(94.574745497895,-2.19762135603939,-0.169650800625656));
#18311=CARTESIAN_POINT('Ctrl Pts',(94.5762192447749,-2.19541801600012,-0.196114355639268));
#18312=CARTESIAN_POINT('Ctrl Pts',(94.5785773159967,-2.19108442030512,-0.238815696861388));
#18313=CARTESIAN_POINT('Ctrl Pts',(94.5794707986488,-2.18925054200563,-0.255080298515061));
#18314=CARTESIAN_POINT('Ctrl Pts',(94.5810516645112,-2.18566261717819,-0.284003865194152));
#18315=CARTESIAN_POINT('Ctrl Pts',(94.5817412426445,-2.18397934293876,-0.296670711041313));
#18316=CARTESIAN_POINT('Ctrl Pts',(94.5831922750453,-2.1801866670565,-0.323427015661422));
#18317=CARTESIAN_POINT('Ctrl Pts',(94.5839528532646,-2.17805062024215,-0.33751214255634));
#18318=CARTESIAN_POINT('Ctrl Pts',(94.585980754515,-2.1719575953012,-0.375219716176894));
#18319=CARTESIAN_POINT('Ctrl Pts',(94.5872401782358,-2.16775182265475,-0.398800358343093));
#18320=CARTESIAN_POINT('Ctrl Pts',(94.5943151576711,-2.14173436744721,-0.53206785181755));
#18321=CARTESIAN_POINT('Ctrl Pts',(94.5998711615385,-2.11198292317703,-0.640042334683499));
#18322=CARTESIAN_POINT('Ctrl Pts',(94.6098883553534,-2.04246581987901,-0.833507129531586));
#18323=CARTESIAN_POINT('Ctrl Pts',(94.6143739435136,-2.00517748515058,-0.919599753557666));
#18324=CARTESIAN_POINT('Ctrl Pts',(94.6234759138139,-1.92025371798433,-1.08575672111937));
#18325=CARTESIAN_POINT('Ctrl Pts',(94.6280830984615,-1.87280386056076,-1.16569473670524));
#18326=CARTESIAN_POINT('Ctrl Pts',(94.633770959352,-1.81188572022221,-1.25495717496773));
#18327=CARTESIAN_POINT('Ctrl Pts',(94.6345789534238,-1.80318169629193,-1.26743170184523));
#18328=CARTESIAN_POINT('Ctrl Pts',(94.6358476899361,-1.7894548422516,-1.28667727845705));
#18329=CARTESIAN_POINT('Ctrl Pts',(94.6363026406733,-1.78452094574,-1.29351151552009));
#18330=CARTESIAN_POINT('Ctrl Pts',(94.6371501145204,-1.77531238233518,-1.30611388783453));
#18331=CARTESIAN_POINT('Ctrl Pts',(94.6375419071523,-1.77104859570609,-1.3118896332484));
#18332=CARTESIAN_POINT('Ctrl Pts',(94.6384528752134,-1.76111882308256,-1.32520391726211));
#18333=CARTESIAN_POINT('Ctrl Pts',(94.6389734211871,-1.75543261148422,-1.33272700550586));
#18334=CARTESIAN_POINT('Ctrl Pts',(94.6406496700567,-1.73707649153843,-1.35669160538816));
#18335=CARTESIAN_POINT('Ctrl Pts',(94.6418171791544,-1.72422288166653,-1.37299025494268));
#18336=CARTESIAN_POINT('Ctrl Pts',(94.6483461243012,-1.65184258107557,-1.46215053888393));
#18337=CARTESIAN_POINT('Ctrl Pts',(94.6539413704332,-1.58793173548193,-1.53131904804282));
#18338=CARTESIAN_POINT('Ctrl Pts',(94.669891758723,-1.39528361127149,-1.71474831573362));
#18339=CARTESIAN_POINT('Ctrl Pts',(94.6802492947213,-1.25729596392934,-1.81835139077675));
#18340=CARTESIAN_POINT('Ctrl Pts',(94.6921566030249,-1.07556145416562,-1.92412306623286));
#18341=CARTESIAN_POINT('Ctrl Pts',(94.6942954122609,-1.0419719778218,-1.94251812638679));
#18342=CARTESIAN_POINT('Ctrl Pts',(94.69726157423,-0.994054931522833,-1.96715882033234));
#18343=CARTESIAN_POINT('Ctrl Pts',(94.6981145982998,-0.980115643916835,
-1.97414092037179));
#18344=CARTESIAN_POINT('Ctrl Pts',(94.6996682424122,-0.954438726629095,
-1.98666331762068));
#18345=CARTESIAN_POINT('Ctrl Pts',(94.7003704187746,-0.942724077335754,
-1.99224891631784));
#18346=CARTESIAN_POINT('Ctrl Pts',(94.7017907621722,-0.918807470638382,
-2.00339427104166));
#18347=CARTESIAN_POINT('Ctrl Pts',(94.7025086578334,-0.906602738075145,
-2.0089468035757));
#18348=CARTESIAN_POINT('Ctrl Pts',(94.7042883342142,-0.876062217245818,
-2.02250618483475));
#18349=CARTESIAN_POINT('Ctrl Pts',(94.7053453933834,-0.85766645096825,-2.03037547516879));
#18350=CARTESIAN_POINT('Ctrl Pts',(94.7094966433949,-0.784448118199279,
-2.06052391041379));
#18351=CARTESIAN_POINT('Ctrl Pts',(94.7125252949487,-0.728842879037055,
-2.0808427294667));
#18352=CARTESIAN_POINT('Ctrl Pts',(94.7205977814119,-0.575800747787049,
-2.12987715655826));
#18353=CARTESIAN_POINT('Ctrl Pts',(94.7255183207916,-0.477089153385412,
-2.15413803855601));
#18354=CARTESIAN_POINT('Ctrl Pts',(94.7371276332037,-0.240453739452461,
-2.19522668619101));
#18355=CARTESIAN_POINT('Ctrl Pts',(94.7437755048809,-0.101935440147125,
-2.20600059452965));
#18356=CARTESIAN_POINT('Ctrl Pts',(94.7520424886914,0.0564468562763539,
-2.20336593864636));
#18357=CARTESIAN_POINT('Ctrl Pts',(94.7530872300339,0.0762297046191279,
-2.2027702298515));
#18358=CARTESIAN_POINT('Ctrl Pts',(94.7546408236654,0.105245319595247,-2.20150517594025));
#18359=CARTESIAN_POINT('Ctrl Pts',(94.7551388072197,0.114486684909912,-2.20104393634964));
#18360=CARTESIAN_POINT('Ctrl Pts',(94.7560281385079,0.130878214525047,-2.20012232102227));
#18361=CARTESIAN_POINT('Ctrl Pts',(94.756418195624,0.138029411599341,-2.19968525341839));
#18362=CARTESIAN_POINT('Ctrl Pts',(94.7572784795002,0.153716898625965,-2.19864966208269));
#18363=CARTESIAN_POINT('Ctrl Pts',(94.7577494858428,0.162251769185203,-2.19803630084633));
#18364=CARTESIAN_POINT('Ctrl Pts',(94.7591228985708,0.18699071275373,-2.19611355803785));
#18365=CARTESIAN_POINT('Ctrl Pts',(94.7600320465024,0.203183808262649,-2.19467459882351));
#18366=CARTESIAN_POINT('Ctrl Pts',(94.7680361211263,0.344320810274916,-2.18055746602971));
#18367=CARTESIAN_POINT('Ctrl Pts',(94.7755839175224,0.467975235483891,-2.15740157320715));
#18368=CARTESIAN_POINT('Ctrl Pts',(94.7927226877972,0.742869450418756,-2.08116949469576));
#18369=CARTESIAN_POINT('Ctrl Pts',(94.8022353651095,0.891694734497508,-2.02188449193232));
#18370=CARTESIAN_POINT('Ctrl Pts',(94.8127596822778,1.05730873895497,-1.93403275758604));
#18371=CARTESIAN_POINT('Ctrl Pts',(94.8143001093834,1.0815514271325,-1.92058092409919));
#18372=CARTESIAN_POINT('Ctrl Pts',(94.8167328458202,1.11982979408872,-1.89838623141298));
#18373=CARTESIAN_POINT('Ctrl Pts',(94.8176355316651,1.13403149155927,-1.88993694299338));
#18374=CARTESIAN_POINT('Ctrl Pts',(94.8192289007036,1.15909106293141,-1.87464358907408));
#18375=CARTESIAN_POINT('Ctrl Pts',(94.8199218584762,1.16998658611627,-1.86786297041886));
#18376=CARTESIAN_POINT('Ctrl Pts',(94.8213645344086,1.19266006286278,-1.85347633414525));
#18377=CARTESIAN_POINT('Ctrl Pts',(94.8221135428954,1.20442593935234,-1.84585230065864));
#18378=CARTESIAN_POINT('Ctrl Pts',(94.8240750096577,1.23521472665582,-1.82548209306741));
#18379=CARTESIAN_POINT('Ctrl Pts',(94.8252804762971,1.25411339267919,-1.81255067331888));
#18380=CARTESIAN_POINT('Ctrl Pts',(94.8312768231741,1.34792013137746,-1.74619367133545));
#18381=CARTESIAN_POINT('Ctrl Pts',(94.8358975204975,1.41963583984997,-1.68840679977406));
#18382=CARTESIAN_POINT('Ctrl Pts',(94.8449594687033,1.55566243577444,-1.56398682131651));
#18383=CARTESIAN_POINT('Ctrl Pts',(94.849391527499,1.61980780340455,-1.49745230921312));
#18384=CARTESIAN_POINT('Ctrl Pts',(94.8553970476742,1.70008183819309,-1.40297512291247));
#18385=CARTESIAN_POINT('Ctrl Pts',(94.8569345307262,1.72005043297731,-1.37842080248154));
#18386=CARTESIAN_POINT('Ctrl Pts',(94.8626328911062,1.79152490284368,-1.28655995975371));
#18387=CARTESIAN_POINT('Ctrl Pts',(94.8668603793646,1.83966084014513,-1.21673466517276));
#18388=CARTESIAN_POINT('Ctrl Pts',(94.8721130381572,1.89145695877538,-1.13147359432857));
#18389=CARTESIAN_POINT('Ctrl Pts',(94.8729116922183,1.89912908514909,-1.11854844101027));
#18390=CARTESIAN_POINT('Ctrl Pts',(94.8741688237443,1.91087619665093,-1.09828891294088));
#18391=CARTESIAN_POINT('Ctrl Pts',(94.874621676791,1.91504265173824,-1.09100779672539));
#18392=CARTESIAN_POINT('Ctrl Pts',(94.8754636883955,1.92266671725094,-1.07750607613209));
#18393=CARTESIAN_POINT('Ctrl Pts',(94.8758521074995,1.92613588463787,-1.07129230323676));
#18394=CARTESIAN_POINT('Ctrl Pts',(94.8767607524788,1.9341413693502,-1.05678874928612));
#18395=CARTESIAN_POINT('Ctrl Pts',(94.8772823973392,1.93865451761071,-1.048486505341));
#18396=CARTESIAN_POINT('Ctrl Pts',(94.8789657872865,1.95296068367755,-1.0217611664808));
#18397=CARTESIAN_POINT('Ctrl Pts',(94.8801394747046,1.96254526295985,-1.00322845825735));
#18398=CARTESIAN_POINT('Ctrl Pts',(94.8867372012658,2.01437870852171,-0.899417392524892));
#18399=CARTESIAN_POINT('Ctrl Pts',(94.8924000728882,2.05132959551711,-0.811613930327904));
#18400=CARTESIAN_POINT('Ctrl Pts',(94.9086214533789,2.13989618315697,-0.556054388239939));
#18401=CARTESIAN_POINT('Ctrl Pts',(94.9191735626596,2.1773438098686,-0.384115138328087));
#18402=CARTESIAN_POINT('Ctrl Pts',(94.9310850295551,2.19740697483563,-0.174040956457307));
#18403=CARTESIAN_POINT('Ctrl Pts',(94.9330720868704,2.19993538459887,-0.138463643182172));
#18404=CARTESIAN_POINT('Ctrl Pts',(94.9359337918393,2.20236468671953,-0.0864566731110639));
#18405=CARTESIAN_POINT('Ctrl Pts',(94.9368295051764,2.20294706206198,-0.0700659111716392));
#18406=CARTESIAN_POINT('Ctrl Pts',(94.9384149387745,2.2036585173826,-0.0408580337970744));
#18407=CARTESIAN_POINT('Ctrl Pts',(94.9391068563871,2.20385884509099,-0.0280435511618437));
#18408=CARTESIAN_POINT('Ctrl Pts',(94.9405517048102,2.20404468462632,-0.00114675610603145));
#18409=CARTESIAN_POINT('Ctrl Pts',(94.9413038794707,2.20400702831426,0.0129351701960996));
#18410=CARTESIAN_POINT('Ctrl Pts',(94.9432835338189,2.20355021233875,0.0502000084250539));
#18411=CARTESIAN_POINT('Ctrl Pts',(94.9445037777823,2.20290018123056,0.073378638528881));
#18412=CARTESIAN_POINT('Ctrl Pts',(94.9507571325891,2.19764897460059,0.193144077679191));
#18413=CARTESIAN_POINT('Ctrl Pts',(94.9556007948011,2.18706093207713,0.289366295581169));
#18414=CARTESIAN_POINT('Ctrl Pts',(94.9670460678092,2.14633691738416,0.519165870379614));
#18415=CARTESIAN_POINT('Ctrl Pts',(94.9735132740383,2.11002345446319,0.65122495560932));
#18416=CARTESIAN_POINT('Ctrl Pts',(94.9836285781819,2.0377162494379,0.842578368128476));
#18417=CARTESIAN_POINT('Ctrl Pts',(94.9870562378527,2.01079654792246,0.904942821402023));
#18418=CARTESIAN_POINT('Ctrl Pts',(94.9913968969472,1.97471083384666,0.97894941946147));
#18419=CARTESIAN_POINT('Ctrl Pts',(94.9921655217908,1.96824969470334,0.991875980380583));
#18420=CARTESIAN_POINT('Ctrl Pts',(94.9933853103976,1.95789713922495,1.01208843483221));
#18421=CARTESIAN_POINT('Ctrl Pts',(94.9938313730318,1.95409097653468,1.01941780375403));
#18422=CARTESIAN_POINT('Ctrl Pts',(94.9946717075392,1.94688539499829,1.03310465649419));
#18423=CARTESIAN_POINT('Ctrl Pts',(94.9950653732984,1.94349587326475,1.03946705473974));
#18424=CARTESIAN_POINT('Ctrl Pts',(94.9959935239273,1.93547084701258,1.05435419036693));
#18425=CARTESIAN_POINT('Ctrl Pts',(94.9965295595233,1.93081018984679,1.06286507230188));
#18426=CARTESIAN_POINT('Ctrl Pts',(94.9983084208148,1.91525232064573,1.09083544535661));
#18427=CARTESIAN_POINT('Ctrl Pts',(94.9995650842185,1.90411625989537,1.11015972330232));
#18428=CARTESIAN_POINT('Ctrl Pts',(95.0026553827308,1.87632760367246,1.15673263157023));
#18429=CARTESIAN_POINT('Ctrl Pts',(95.0045034541841,1.859372564361,1.18379438500978));
#18430=CARTESIAN_POINT('Ctrl Pts',(95.0122371096884,1.78677878771326,1.29425155196647));
#18431=CARTESIAN_POINT('Ctrl Pts',(95.0182866652785,1.72607166508914,1.37416913101112));
#18432=CARTESIAN_POINT('Ctrl Pts',(95.0328681820659,1.5662869875503,1.5571514175172));
#18433=CARTESIAN_POINT('Ctrl Pts',(95.0413139952279,1.46220806014156,1.65527456326024));
#18434=CARTESIAN_POINT('Ctrl Pts',(95.051075126406,1.32482885774414,1.76164893967077));
#18435=CARTESIAN_POINT('Ctrl Pts',(95.0527982697611,1.29989972305135,1.78012340508014));
#18436=CARTESIAN_POINT('Ctrl Pts',(95.0553742590352,1.26160864439989,1.80726664890969));
#18437=CARTESIAN_POINT('Ctrl Pts',(95.0562420197389,1.24852990153853,1.81632657183962));
#18438=CARTESIAN_POINT('Ctrl Pts',(95.057794578453,1.22480897708247,1.8323812657761));
#18439=CARTESIAN_POINT('Ctrl Pts',(95.0584812823748,1.21420219599957,1.83942685916755));
#18440=CARTESIAN_POINT('Ctrl Pts',(95.0599442115389,1.19136254978204,1.85431453413357));
#18441=CARTESIAN_POINT('Ctrl Pts',(95.0607193619697,1.17911195102925,1.86212838904119));
#18442=CARTESIAN_POINT('Ctrl Pts',(95.0628311415837,1.1453365721306,1.88320452680582));
#18443=CARTESIAN_POINT('Ctrl Pts',(95.0641586604965,1.12365913181226,1.89621870522438));
#18444=CARTESIAN_POINT('Ctrl Pts',(95.0732955525266,0.971499688881277,1.9840427023134));
#18445=CARTESIAN_POINT('Ctrl Pts',(95.0806084984028,0.833881793724874,2.04569894083342));
#18446=CARTESIAN_POINT('Ctrl Pts',(95.0919755234633,0.610576225909772,2.11943240375127));
#18447=CARTESIAN_POINT('Ctrl Pts',(95.0960573438333,0.528645867197792,2.1413382577356));
#18448=CARTESIAN_POINT('Ctrl Pts',(95.103286690977,0.386007031158793,2.1707890096286));
#18449=CARTESIAN_POINT('Ctrl Pts',(95.1063719261145,0.325872097147621,2.18062664968732));
#18450=CARTESIAN_POINT('Ctrl Pts',(95.1103772907329,0.25032707108405,2.18979068910146));
#18451=CARTESIAN_POINT('Ctrl Pts',(95.1111844849624,0.235224001110319,2.19146447575686));
#18452=CARTESIAN_POINT('Ctrl Pts',(95.1124522278693,0.211721613711599,2.19382336383564));
#18453=CARTESIAN_POINT('Ctrl Pts',(95.1129069992533,0.203333360523734,2.19461671668196));
#18454=CARTESIAN_POINT('Ctrl Pts',(95.1137506618996,0.187856377468746,2.19599102178044));
#18455=CARTESIAN_POINT('Ctrl Pts',(95.1141387878109,0.180769143098662,2.19658578222223));
#18456=CARTESIAN_POINT('Ctrl Pts',(95.1149152780157,0.166654566063787,2.19770150590659));
#18457=CARTESIAN_POINT('Ctrl Pts',(95.1153035821304,0.159627434170662,2.19822308533632));
#18458=CARTESIAN_POINT('Ctrl Pts',(95.1162074481433,0.143338726683818,2.19935357706634));
#18459=CARTESIAN_POINT('Ctrl Pts',(95.1167242955759,0.134075626027717,2.19993769638116));
#18460=CARTESIAN_POINT('Ctrl Pts',(95.1195564510705,0.0835752989115121,
2.20280205199079));
#18461=CARTESIAN_POINT('Ctrl Pts',(95.1219242869929,0.0422862894867362,
2.20398120245318));
#18462=CARTESIAN_POINT('Ctrl Pts',(95.1243288921836,0.000991366063952221,
2.20399977704022));
#18463=CARTESIAN_POINT('Ctrl Pts',(95.1243288469655,0.000992142605052562,
2.20399977669079));
#18464=CARTESIAN_POINT('Ctrl Pts',(95.1243481046162,0.000661425794219861,
2.20399992556478));
#18465=CARTESIAN_POINT('Ctrl Pts',(95.1243673644587,0.000330711594234764,
2.204));
#18466=CARTESIAN_POINT('Ctrl Pts',(95.1243866264839,2.95873024051195E-11,
2.204));
#18467=CARTESIAN_POINT('Origin',(66.9212607628943,0.,0.));
#18468=CARTESIAN_POINT('',(95.9829026914895,-1.13898760397551E-11,2.204));
#18469=CARTESIAN_POINT('',(95.8777130322977,9.44243789243157E-12,2.204));
#18470=CARTESIAN_POINT('',(66.9212607628943,-2.69912154532077E-16,2.204));
#18471=CARTESIAN_POINT('Ctrl Pts',(95.9829026914895,-1.13898760397551E-11,
2.204));
#18472=CARTESIAN_POINT('Ctrl Pts',(95.9828788298517,0.000477678869200619,
2.204));
#18473=CARTESIAN_POINT('Ctrl Pts',(95.9828549715523,0.000955359704270702,
2.20399984473618));
#18474=CARTESIAN_POINT('Ctrl Pts',(95.9772330995163,0.113530410574079,2.20392664806559));
#18475=CARTESIAN_POINT('Ctrl Pts',(95.971843390864,0.225462406806485,2.19530176314732));
#18476=CARTESIAN_POINT('Ctrl Pts',(95.960748388197,0.452160190387588,2.16030593424989));
#18477=CARTESIAN_POINT('Ctrl Pts',(95.9550547837466,0.566442579419279,2.13319190341888));
#18478=CARTESIAN_POINT('Ctrl Pts',(95.9479704766969,0.695808852201622,2.09136698605005));
#18479=CARTESIAN_POINT('Ctrl Pts',(95.9469854486833,0.713531039618399,2.08538707198984));
#18480=CARTESIAN_POINT('Ctrl Pts',(95.9454995899027,0.739819876967249,2.07614222474404));
#18481=CARTESIAN_POINT('Ctrl Pts',(95.9450080326983,0.748446153979837,2.07304807864895));
#18482=CARTESIAN_POINT('Ctrl Pts',(95.9441552683583,0.763283024209296,2.06762158867299));
#18483=CARTESIAN_POINT('Ctrl Pts',(95.9437955483123,0.769502913561527,2.06531481198765));
#18484=CARTESIAN_POINT('Ctrl Pts',(95.9430286584377,0.782678114204441,2.06036073396123));
#18485=CARTESIAN_POINT('Ctrl Pts',(95.9426210487632,0.789630580475892,2.05770622947755));
#18486=CARTESIAN_POINT('Ctrl Pts',(95.9415882394253,0.807124976781946,2.05092501920776));
#18487=CARTESIAN_POINT('Ctrl Pts',(95.940960382653,0.817648699440852,2.04675224577705));
#18488=CARTESIAN_POINT('Ctrl Pts',(95.9384350863003,0.859557583582711,2.02976011459988));
#18489=CARTESIAN_POINT('Ctrl Pts',(95.9365038151161,0.89067581866469,2.01629900957249));
#18490=CARTESIAN_POINT('Ctrl Pts',(95.9312016022936,0.974021133981133,1.97793971267486));
#18491=CARTESIAN_POINT('Ctrl Pts',(95.9277799541229,1.02559749774177,1.95169457898942));
#18492=CARTESIAN_POINT('Ctrl Pts',(95.9160056719715,1.19772130709342,1.85539963625697));
#18493=CARTESIAN_POINT('Ctrl Pts',(95.9075499420374,1.31264472648618,1.7759541265129));
#18494=CARTESIAN_POINT('Ctrl Pts',(95.8948546686544,1.47884266353129,1.63606184903826));
#18495=CARTESIAN_POINT('Ctrl Pts',(95.8904052116827,1.53569690762821,1.58281744223646));
#18496=CARTESIAN_POINT('Ctrl Pts',(95.884836772622,1.60515496398002,1.51049546387426));
#18497=CARTESIAN_POINT('Ctrl Pts',(95.8836019046699,1.62044284947127,1.49408300602855));
#18498=CARTESIAN_POINT('Ctrl Pts',(95.8816229298707,1.64474782850392,1.46717817867799));
#18499=CARTESIAN_POINT('Ctrl Pts',(95.8808722494358,1.65392105181594,1.45682956929318));
#18500=CARTESIAN_POINT('Ctrl Pts',(95.8794389704193,1.67134302971768,1.43679860675478));
#18501=CARTESIAN_POINT('Ctrl Pts',(95.8787557726136,1.67960653277266,1.42712986929033));
#18502=CARTESIAN_POINT('Ctrl Pts',(95.8771811372737,1.69855321179957,1.40456872547964));
#18503=CARTESIAN_POINT('Ctrl Pts',(95.8762922557781,1.70917416944192,1.3916249485023));
#18504=CARTESIAN_POINT('Ctrl Pts',(95.8734499402949,1.74288091317044,1.34957843215756));
#18505=CARTESIAN_POINT('Ctrl Pts',(95.8715197610336,1.76537940108509,1.32001197042428));
#18506=CARTESIAN_POINT('Ctrl Pts',(95.8637313666677,1.85428498454624,1.19683477041537));
#18507=CARTESIAN_POINT('Ctrl Pts',(95.8581153579943,1.91408239820586,1.0986709879389));
#18508=CARTESIAN_POINT('Ctrl Pts',(95.8457792044542,2.02924036487385,0.871431735969079));
#18509=CARTESIAN_POINT('Ctrl Pts',(95.8391169559389,2.0804708370472,0.740839780797122));
#18510=CARTESIAN_POINT('Ctrl Pts',(95.8303830579762,2.12728246153167,0.577233542046017));
#18511=CARTESIAN_POINT('Ctrl Pts',(95.8288080015182,2.13499663890228,0.548013147820725));
#18512=CARTESIAN_POINT('Ctrl Pts',(95.8266075336666,2.14473689035551,0.507783955018259));
#18513=CARTESIAN_POINT('Ctrl Pts',(95.8260092080454,2.14728382352938,0.496903455824378));
#18514=CARTESIAN_POINT('Ctrl Pts',(95.8250460247891,2.15121999231037,0.479492559427847));
#18515=CARTESIAN_POINT('Ctrl Pts',(95.8246841458569,2.15266251801091,0.472974260372433));
#18516=CARTESIAN_POINT('Ctrl Pts',(95.8239179273568,2.15563984879748,0.459224875658199));
#18517=CARTESIAN_POINT('Ctrl Pts',(95.8235131946761,2.157167919286,0.451992486138058));
#18518=CARTESIAN_POINT('Ctrl Pts',(95.822496695825,2.16089569634518,0.433899281488422));
#18519=CARTESIAN_POINT('Ctrl Pts',(95.8218824355277,2.16304991204809,0.42302938946607));
#18520=CARTESIAN_POINT('Ctrl Pts',(95.8194794057673,2.17110202893434,0.380729082836426));
#18521=CARTESIAN_POINT('Ctrl Pts',(95.8176606780988,2.17639730140451,0.349189384573342));
#18522=CARTESIAN_POINT('Ctrl Pts',(95.8127577551507,2.18864603562437,0.265061653354419));
#18523=CARTESIAN_POINT('Ctrl Pts',(95.8096309306682,2.19439031154624,0.212319829583095));
#18524=CARTESIAN_POINT('Ctrl Pts',(95.7971070184038,2.20960255166768,0.00256671632292191));
#18525=CARTESIAN_POINT('Ctrl Pts',(95.7875393528914,2.20415722066994,-0.15507799154341));
#18526=CARTESIAN_POINT('Ctrl Pts',(95.7743943310034,2.17225322307569,-0.379058427748882));
#18527=CARTESIAN_POINT('Ctrl Pts',(95.7704708080942,2.15933286616092,-0.446824770169614));
#18528=CARTESIAN_POINT('Ctrl Pts',(95.7654504441312,2.13822707356381,-0.534851470617449));
#18529=CARTESIAN_POINT('Ctrl Pts',(95.7642641741997,2.13289100953263,-0.55574913577905));
#18530=CARTESIAN_POINT('Ctrl Pts',(95.7623435676437,2.123679689425,-0.589734460311962));
#18531=CARTESIAN_POINT('Ctrl Pts',(95.7616033493435,2.11998818038015,-0.602870038866647));
#18532=CARTESIAN_POINT('Ctrl Pts',(95.760177175874,2.11260163575163,-0.628246603148619));
#18533=CARTESIAN_POINT('Ctrl Pts',(95.7594907658293,2.10892159730474,-0.640491351779439));
#18534=CARTESIAN_POINT('Ctrl Pts',(95.7578895911733,2.1000444964434,-0.66912226191492));
#18535=CARTESIAN_POINT('Ctrl Pts',(95.756977668929,2.09476182874159,-0.685481138923474));
#18536=CARTESIAN_POINT('Ctrl Pts',(95.7539758941104,2.07662344326546,-0.739481658425887));
#18537=CARTESIAN_POINT('Ctrl Pts',(95.7519132345112,2.06293987069779,-0.776838073883258));
#18538=CARTESIAN_POINT('Ctrl Pts',(95.741922073855,1.99078526391338,-0.958442731523179));
#18539=CARTESIAN_POINT('Ctrl Pts',(95.734474716815,1.91816123209685,-1.0965852934875));
#18540=CARTESIAN_POINT('Ctrl Pts',(95.7261011386309,1.82198430786955,-1.24027704862635));
#18541=CARTESIAN_POINT('Ctrl Pts',(95.7252638884385,1.81221452863861,-1.25450885662443));
#18542=CARTESIAN_POINT('Ctrl Pts',(95.719542317405,1.74451276575315,-1.35068976370314));
#18543=CARTESIAN_POINT('Ctrl Pts',(95.7145881457256,1.68121490013588,-1.42870565251597));
#18544=CARTESIAN_POINT('Ctrl Pts',(95.7085086333395,1.60249588267664,-1.5132259905181));
#18545=CARTESIAN_POINT('Ctrl Pts',(95.707703080167,1.59204681767393,-1.52421548918479));
#18546=CARTESIAN_POINT('Ctrl Pts',(95.7064400485751,1.57565635863231,-1.54110125604584));
#18547=CARTESIAN_POINT('Ctrl Pts',(95.7059883475131,1.56979318012819,-1.54707317500567));
#18548=CARTESIAN_POINT('Ctrl Pts',(95.7051483621836,1.55889164258052,-1.55805111944311));
#18549=CARTESIAN_POINT('Ctrl Pts',(95.7047608123871,1.55386293597412,-1.56306635043527));
#18550=CARTESIAN_POINT('Ctrl Pts',(95.7038620788419,1.54220287107331,-1.57458329405822));
#18551=CARTESIAN_POINT('Ctrl Pts',(95.7033495828948,1.53555459518991,-1.58106746354528));
#18552=CARTESIAN_POINT('Ctrl Pts',(95.7017088200238,1.51426471523994,-1.60157088131654));
#18553=CARTESIAN_POINT('Ctrl Pts',(95.7005693169641,1.49947098748378,-1.61542985417944));
#18554=CARTESIAN_POINT('Ctrl Pts',(95.6943003445732,1.41790414396953,-1.68975701573796));
#18555=CARTESIAN_POINT('Ctrl Pts',(95.6889548297688,1.34766744132494,-1.74628769886602));
#18556=CARTESIAN_POINT('Ctrl Pts',(95.6739828307553,1.14375280433932,-1.89076571931951));
#18557=CARTESIAN_POINT('Ctrl Pts',(95.6643276363342,1.00364508545977,-1.96872390992964));
#18558=CARTESIAN_POINT('Ctrl Pts',(95.6522988591321,0.810118905627756,-2.05032635989805));
#18559=CARTESIAN_POINT('Ctrl Pts',(95.6494747267164,0.763256919178165,-2.06822877608177));
#18560=CARTESIAN_POINT('Ctrl Pts',(95.6456357597286,0.69755139693683,-2.09079201087649));
#18561=CARTESIAN_POINT('Ctrl Pts',(95.6445761751776,0.679198588308657,-2.09682581425617));
#18562=CARTESIAN_POINT('Ctrl Pts',(95.6428789795635,0.649455411325713,-2.106172901717));
#18563=CARTESIAN_POINT('Ctrl Pts',(95.6422364539973,0.638113766044681,-2.10963680583228));
#18564=CARTESIAN_POINT('Ctrl Pts',(95.6409025675322,0.614400945242074,-2.11667032108227));
#18565=CARTESIAN_POINT('Ctrl Pts',(95.6402117675341,0.602025311799606,-2.12022340882817));
#18566=CARTESIAN_POINT('Ctrl Pts',(95.6385780055691,0.572535139050384,-2.12841111472538));
#18567=CARTESIAN_POINT('Ctrl Pts',(95.6376382380577,0.555394275571141,-2.13294809643092));
#18568=CARTESIAN_POINT('Ctrl Pts',(95.6344342076581,0.496367943449949,-2.14781185551503));
#18569=CARTESIAN_POINT('Ctrl Pts',(95.6322026140006,0.454233855180053,-2.15711585862535));
#18570=CARTESIAN_POINT('Ctrl Pts',(95.6267873507527,0.349832029120907,-2.1769747788754));
#18571=CARTESIAN_POINT('Ctrl Pts',(95.623644859853,0.287331454366506,-2.18610223600651));
#18572=CARTESIAN_POINT('Ctrl Pts',(95.6161054336892,0.134532717289035,-2.20174930547751));
#18573=CARTESIAN_POINT('Ctrl Pts',(95.6117634442917,0.044059877445082,-2.20541562124689));
#18574=CARTESIAN_POINT('Ctrl Pts',(95.6058453996764,-0.0780494992300799,
-2.20284533234442));
#18575=CARTESIAN_POINT('Ctrl Pts',(95.6043058133446,-0.109698663752618,
-2.20149618041527));
#18576=CARTESIAN_POINT('Ctrl Pts',(95.5986592491845,-0.2247192225508,-2.19410654689001));
#18577=CARTESIAN_POINT('Ctrl Pts',(95.5944858612555,-0.307751210250835,
-2.1840075083954));
#18578=CARTESIAN_POINT('Ctrl Pts',(95.5892997238766,-0.404670569433291,
-2.16658253927671));
#18579=CARTESIAN_POINT('Ctrl Pts',(95.5885075836227,-0.41931317222477,-2.1637963418094));
#18580=CARTESIAN_POINT('Ctrl Pts',(95.5872612140708,-0.442074753300329,
-2.15922555388672));
#18581=CARTESIAN_POINT('Ctrl Pts',(95.5868125230817,-0.450214061229815,
-2.15754313387671));
#18582=CARTESIAN_POINT('Ctrl Pts',(95.5859787511895,-0.465232241058508,
-2.15435014827385));
#18583=CARTESIAN_POINT('Ctrl Pts',(95.585594400985,-0.472113615061271,-2.1528526028219));
#18584=CARTESIAN_POINT('Ctrl Pts',(95.5846964019476,-0.488096102725699,
-2.14929413314906));
#18585=CARTESIAN_POINT('Ctrl Pts',(95.5841813767188,-0.497191399158086,
-2.14720836958512));
#18586=CARTESIAN_POINT('Ctrl Pts',(95.5825242800639,-0.526240568349298,
-2.14035225542374));
#18587=CARTESIAN_POINT('Ctrl Pts',(95.5813706672503,-0.546140636243568,
-2.13536115372221));
#18588=CARTESIAN_POINT('Ctrl Pts',(95.5749483671129,-0.655360317659839,
-2.10634140111173));
#18589=CARTESIAN_POINT('Ctrl Pts',(95.5694527341025,-0.743162466192057,
-2.07698771908025));
#18590=CARTESIAN_POINT('Ctrl Pts',(95.5539061634405,-0.983485103588377,
-1.97945012509756));
#18591=CARTESIAN_POINT('Ctrl Pts',(95.5438407265759,-1.13051297393192,-1.89932112531321));
#18592=CARTESIAN_POINT('Ctrl Pts',(95.5318979071458,-1.30224624603176,-1.77865576549699));
#18593=CARTESIAN_POINT('Ctrl Pts',(95.5294896912767,-1.33666937037276,-1.75293381917311));
#18594=CARTESIAN_POINT('Ctrl Pts',(95.5261169977226,-1.38456807387419,-1.71491054161252));
#18595=CARTESIAN_POINT('Ctrl Pts',(95.5251208107109,-1.39867547277355,-1.70342415939696));
#18596=CARTESIAN_POINT('Ctrl Pts',(95.5234341090007,-1.42248660896125,-1.68354163184494));
#18597=CARTESIAN_POINT('Ctrl Pts',(95.5227400899828,-1.43226202674004,-1.67523314059028));
#18598=CARTESIAN_POINT('Ctrl Pts',(95.5213337894339,-1.45202172090621,-1.65813924831427));
#18599=CARTESIAN_POINT('Ctrl Pts',(95.5206217978757,-1.46200014760925,-1.64934787835859));
#18600=CARTESIAN_POINT('Ctrl Pts',(95.5188523860982,-1.48672819769768,-1.62716078778031));
#18601=CARTESIAN_POINT('Ctrl Pts',(95.5177996781805,-1.50137704831877,-1.61365422460098));
#18602=CARTESIAN_POINT('Ctrl Pts',(95.5136359095201,-1.55902772957845,-1.55903424355645));
#18603=CARTESIAN_POINT('Ctrl Pts',(95.5105912748449,-1.60054204983427,-1.5163842403494));
#18604=CARTESIAN_POINT('Ctrl Pts',(95.5024446440686,-1.70888344084178,-1.39566555941648));
#18605=CARTESIAN_POINT('Ctrl Pts',(95.4974696147281,-1.7720602108341,-1.31452240006163));
#18606=CARTESIAN_POINT('Ctrl Pts',(95.4858758005733,-1.90584587988259,-1.11542754964171));
#18607=CARTESIAN_POINT('Ctrl Pts',(95.4792935692208,-1.97154078234737,-0.994708786994209));
#18608=CARTESIAN_POINT('Ctrl Pts',(95.4711020069243,-2.03340958794017,-0.850444247370904));
#18609=CARTESIAN_POINT('Ctrl Pts',(95.4700543057658,-2.04098571409772,-0.832098089668565));
#18610=CARTESIAN_POINT('Ctrl Pts',(95.468505241796,-2.05167649511576,-0.805184811190546));
#18611=CARTESIAN_POINT('Ctrl Pts',(95.4680149187935,-2.05498761992263,-0.796696238730226));
#18612=CARTESIAN_POINT('Ctrl Pts',(95.4671369146973,-2.06078521058513,-0.781556608820664));
#18613=CARTESIAN_POINT('Ctrl Pts',(95.4667504611938,-2.06329230078625,-0.774913735121403));
#18614=CARTESIAN_POINT('Ctrl Pts',(95.4659034086266,-2.06868979847421,-0.760400427952536));
#18615=CARTESIAN_POINT('Ctrl Pts',(95.4654421050132,-2.07156737125649,-0.752525690405685));
#18616=CARTESIAN_POINT('Ctrl Pts',(95.4641113287956,-2.07969458913825,-0.729884929413623));
#18617=CARTESIAN_POINT('Ctrl Pts',(95.4632356507201,-2.08483166237382,-0.71507936986997));
#18618=CARTESIAN_POINT('Ctrl Pts',(95.4612172302294,-2.09620773832884,-0.681127446893309));
#18619=CARTESIAN_POINT('Ctrl Pts',(95.4600695911161,-2.10234304626968,-0.661947992250309));
#18620=CARTESIAN_POINT('Ctrl Pts',(95.4561945063687,-2.12199067125946,-0.597497714309787));
#18621=CARTESIAN_POINT('Ctrl Pts',(95.4534214199588,-2.13430960194535,-0.551878597772534));
#18622=CARTESIAN_POINT('Ctrl Pts',(95.4448960935618,-2.1672901412406,-0.41203262207989));
#18623=CARTESIAN_POINT('Ctrl Pts',(95.439062859636,-2.18324229816694,-0.316812846154468));
#18624=CARTESIAN_POINT('Ctrl Pts',(95.4253507254016,-2.2062190450609,-0.0886728181536196));
#18625=CARTESIAN_POINT('Ctrl Pts',(95.4175717140012,-2.20755480215899,0.0444581155629141));
#18626=CARTESIAN_POINT('Ctrl Pts',(95.4088141015528,-2.19493515189288,0.201165496283699));
#18627=CARTESIAN_POINT('Ctrl Pts',(95.407471282794,-2.19258085752587,0.225382182350168));
#18628=CARTESIAN_POINT('Ctrl Pts',(95.4053551211063,-2.18819855392625,0.263836463201095));
#18629=CARTESIAN_POINT('Ctrl Pts',(95.4045736602767,-2.18643140608747,0.278101260277108));
#18630=CARTESIAN_POINT('Ctrl Pts',(95.4031215665938,-2.18286858927177,0.304723853630748));
#18631=CARTESIAN_POINT('Ctrl Pts',(95.4024498823252,-2.18110720594006,0.317085587986598));
#18632=CARTESIAN_POINT('Ctrl Pts',(95.4009410074096,-2.17689393128738,0.344957027060245));
#18633=CARTESIAN_POINT('Ctrl Pts',(95.4001057778675,-2.17438114415292,0.36045692648497));
#18634=CARTESIAN_POINT('Ctrl Pts',(95.397611240752,-2.16633291634213,0.406950713635804));
#18635=CARTESIAN_POINT('Ctrl Pts',(95.3959677169264,-2.16029870135175,0.437854815330427));
#18636=CARTESIAN_POINT('Ctrl Pts',(95.3922146820598,-2.14483321671233,0.508928449400112));
#18637=CARTESIAN_POINT('Ctrl Pts',(95.390119623358,-2.13493198887868,0.548983921417049));
#18638=CARTESIAN_POINT('Ctrl Pts',(95.3825820270884,-2.09477434920969,0.693854952460232));
#18639=CARTESIAN_POINT('Ctrl Pts',(95.3773179076906,-2.05787242978463,0.796666114248553));
#18640=CARTESIAN_POINT('Ctrl Pts',(95.3658907633888,-1.96172497225474,1.01265245630798));
#18641=CARTESIAN_POINT('Ctrl Pts',(95.3597452632532,-1.89996253176276,1.12426208386168));
#18642=CARTESIAN_POINT('Ctrl Pts',(95.3520460566563,-1.81755857001209,1.24680049822258));
#18643=CARTESIAN_POINT('Ctrl Pts',(95.350971943148,-1.80596232214276,1.26353894696805));
#18644=CARTESIAN_POINT('Ctrl Pts',(95.3493909418991,-1.78878998135921,1.28760674525041));
#18645=CARTESIAN_POINT('Ctrl Pts',(95.348895746397,-1.78339693051318,1.29506606393181));
#18646=CARTESIAN_POINT('Ctrl Pts',(95.3480124187299,-1.77375603906876,1.30822630161916));
#18647=CARTESIAN_POINT('Ctrl Pts',(95.3476255735493,-1.7695271201249,1.31394075670797));
#18648=CARTESIAN_POINT('Ctrl Pts',(95.3467818448893,-1.76029024742898,1.32629688646903));
#18649=CARTESIAN_POINT('Ctrl Pts',(95.3463243037234,-1.75527239636436,1.33293060440226));
#18650=CARTESIAN_POINT('Ctrl Pts',(95.3450149921736,-1.74088392023998,1.3517303716658));
#18651=CARTESIAN_POINT('Ctrl Pts',(95.344157312315,-1.73142370736625,1.36382687317468));
#18652=CARTESIAN_POINT('Ctrl Pts',(95.3369273091094,-1.65131025305964,1.46408859531355));
#18653=CARTESIAN_POINT('Ctrl Pts',(95.3301804322812,-1.57410595504838,1.54679239377701));
#18654=CARTESIAN_POINT('Ctrl Pts',(95.3127948679752,-1.3608553742288,1.74266270100023));
#18655=CARTESIAN_POINT('Ctrl Pts',(95.302217609042,-1.21688933528131,1.8460772132719));
#18656=CARTESIAN_POINT('Ctrl Pts',(95.2908520154223,-1.0391345974718,1.94383706267887));
#18657=CARTESIAN_POINT('Ctrl Pts',(95.2893974875975,-1.01593989504199,1.95605967473525));
#18658=CARTESIAN_POINT('Ctrl Pts',(95.2870684537167,-0.978080847492173,
1.97515463042978));
#18659=CARTESIAN_POINT('Ctrl Pts',(95.2861850352415,-0.963549666854866,
1.9822840405858));
#18660=CARTESIAN_POINT('Ctrl Pts',(95.2846212311532,-0.937525699437962,
1.99469835439482));
#18661=CARTESIAN_POINT('Ctrl Pts',(95.283938705088,-0.926063585665992,2.00004555116683));
#18662=CARTESIAN_POINT('Ctrl Pts',(95.2825019375973,-0.901718178386317,
2.01114877970292));
#18663=CARTESIAN_POINT('Ctrl Pts',(95.2817485597674,-0.888824322936559,
2.01688036902577));
#18664=CARTESIAN_POINT('Ctrl Pts',(95.2797389684467,-0.854093952055924,
2.03192100436055));
#18665=CARTESIAN_POINT('Ctrl Pts',(95.2784905193784,-0.832160303015017,
2.04100189483063));
#18666=CARTESIAN_POINT('Ctrl Pts',(95.2715036968061,-0.707489657566127,
2.09027365424749));
#18667=CARTESIAN_POINT('Ctrl Pts',(95.2660175869942,-0.601991578221309,
2.123062732397));
#18668=CARTESIAN_POINT('Ctrl Pts',(95.2525226581781,-0.332278619496873,
2.18515625133316));
#18669=CARTESIAN_POINT('Ctrl Pts',(95.2447107407989,-0.166398251888413,
2.2039999999985));
#18670=CARTESIAN_POINT('Ctrl Pts',(95.2361698906488,-1.99362401587244E-11,
2.204));
#18671=CARTESIAN_POINT('Ctrl Pts',(95.1243866264839,2.95869231892176E-11,
2.204));
#18672=CARTESIAN_POINT('Ctrl Pts',(95.1365232181435,-0.208374310327999,
2.2040000000028));
#18673=CARTESIAN_POINT('Ctrl Pts',(95.1493967605743,-0.41570994031362,2.17445261716368));
#18674=CARTESIAN_POINT('Ctrl Pts',(95.164981094345,-0.67481589797497,2.09905037989901));
#18675=CARTESIAN_POINT('Ctrl Pts',(95.1684599173385,-0.733054288206009,
2.07942815222445));
#18676=CARTESIAN_POINT('Ctrl Pts',(95.1729812526661,-0.809317108816974,
2.05012986019935));
#18677=CARTESIAN_POINT('Ctrl Pts',(95.1740940190293,-0.828132437153745,
2.04260209820613));
#18678=CARTESIAN_POINT('Ctrl Pts',(95.1759314248133,-0.859269290060516,
2.02964368339487));
#18679=CARTESIAN_POINT('Ctrl Pts',(95.1766609000501,-0.871649394051703,
2.02435780916168));
#18680=CARTESIAN_POINT('Ctrl Pts',(95.1780841027412,-0.895834899339802,
2.01376843247683));
#18681=CARTESIAN_POINT('Ctrl Pts',(95.1787780937438,-0.907643533002457,
2.00847372235246));
#18682=CARTESIAN_POINT('Ctrl Pts',(95.1804437470377,-0.936016495251098,
1.99545062484916));
#18683=CARTESIAN_POINT('Ctrl Pts',(95.1814118318033,-0.952532795577292,
1.98761952493749));
#18684=CARTESIAN_POINT('Ctrl Pts',(95.1846193798058,-1.00731505594976,1.96080516139552));
#18685=CARTESIAN_POINT('Ctrl Pts',(95.1868274237,-1.0451274403687,1.94091459021816));
#18686=CARTESIAN_POINT('Ctrl Pts',(95.1975079459947,-1.22781502606079,1.83792682001616));
#18687=CARTESIAN_POINT('Ctrl Pts',(95.2054300586328,-1.36349433174788,1.73965219684265));
#18688=CARTESIAN_POINT('Ctrl Pts',(95.218372533116,-1.5599291579796,1.56014640895244));
#18689=CARTESIAN_POINT('Ctrl Pts',(95.2232619555242,-1.62848229692825,1.48844790720758));
#18690=CARTESIAN_POINT('Ctrl Pts',(95.2293253611694,-1.70245547567915,1.39983176247767));
#18691=CARTESIAN_POINT('Ctrl Pts',(95.230193102341,-1.71279823376751,1.38715744922183));
#18692=CARTESIAN_POINT('Ctrl Pts',(95.2315305488298,-1.72834773036982,1.36766359372778));
#18693=CARTESIAN_POINT('Ctrl Pts',(95.2319932686743,-1.73365753174243,1.36092657417188));
#18694=CARTESIAN_POINT('Ctrl Pts',(95.232847531939,-1.74332881656237,1.34850730306119));
#18695=CARTESIAN_POINT('Ctrl Pts',(95.2332382396786,-1.74770208567038,1.34283458573826));
#18696=CARTESIAN_POINT('Ctrl Pts',(95.2341366496679,-1.75764470248694,1.32980683243689));
#18697=CARTESIAN_POINT('Ctrl Pts',(95.2346455866618,-1.76319556233371,1.32243809476048));
#18698=CARTESIAN_POINT('Ctrl Pts',(95.2362476175645,-1.78042146999106,1.29926953710171));
#18699=CARTESIAN_POINT('Ctrl Pts',(95.2373511489964,-1.79193132926847,1.2833487435218));
#18700=CARTESIAN_POINT('Ctrl Pts',(95.2464557668316,-1.88417171057394,1.15209857621129));
#18701=CARTESIAN_POINT('Ctrl Pts',(95.2549873615087,-1.95389018917339,1.02943786771139));
#18702=CARTESIAN_POINT('Ctrl Pts',(95.2660609338512,-2.02934889534617,0.860976278647757));
#18703=CARTESIAN_POINT('Ctrl Pts',(95.2686815784102,-2.04606950036018,0.820449178914159));
#18704=CARTESIAN_POINT('Ctrl Pts',(95.2755153672847,-2.08682444937102,0.71265617668105));
#18705=CARTESIAN_POINT('Ctrl Pts',(95.2796878499968,-2.10881859467256,0.644670930322019));
#18706=CARTESIAN_POINT('Ctrl Pts',(95.2864528238454,-2.13977971642495,0.530262010079944));
#18707=CARTESIAN_POINT('Ctrl Pts',(95.2890984373194,-2.15062464293121,0.484405982417027));
#18708=CARTESIAN_POINT('Ctrl Pts',(95.2927144408188,-2.16365750662576,0.420169023220054));
#18709=CARTESIAN_POINT('Ctrl Pts',(95.2937241813549,-2.16709614046601,0.402057410326371));
#18710=CARTESIAN_POINT('Ctrl Pts',(95.2954390690828,-2.1725889372381,0.371005260783025));
#18711=CARTESIAN_POINT('Ctrl Pts',(95.2961477585141,-2.17475564646544,0.358085858809067));
#18712=CARTESIAN_POINT('Ctrl Pts',(95.2974918891146,-2.17866657752132,0.333420064421395));
#18713=CARTESIAN_POINT('Ctrl Pts',(95.2981279575773,-2.18043129521987,0.321677431286295));
#18714=CARTESIAN_POINT('Ctrl Pts',(95.2996096601292,-2.18433916622332,0.29416277160753));
#18715=CARTESIAN_POINT('Ctrl Pts',(95.3004528845243,-2.18640655376888,0.278380546663963));
#18716=CARTESIAN_POINT('Ctrl Pts',(95.3033742173839,-2.19301695926417,0.223289782382924));
#18717=CARTESIAN_POINT('Ctrl Pts',(95.3054246690753,-2.19667239832511,0.183881306837095));
#18718=CARTESIAN_POINT('Ctrl Pts',(95.31615093487,-2.21042544835393,-0.0255912422011547));
#18719=CARTESIAN_POINT('Ctrl Pts',(95.3242345960981,-2.20184179492465,-0.196291835706937));
#18720=CARTESIAN_POINT('Ctrl Pts',(95.3370656479402,-2.15821786981221,-0.456579914631635));
#18721=CARTESIAN_POINT('Ctrl Pts',(95.3416745219566,-2.13689435998858,-0.547767171442031));
#18722=CARTESIAN_POINT('Ctrl Pts',(95.3476275518187,-2.10385812124239,-0.657134446949495));
#18723=CARTESIAN_POINT('Ctrl Pts',(95.3487191855103,-2.09759238200129,-0.676868387191782));
#18724=CARTESIAN_POINT('Ctrl Pts',(95.3503296111129,-2.08807260963721,-0.705448459633346));
#18725=CARTESIAN_POINT('Ctrl Pts',(95.3508363710408,-2.08503820220943,-0.714367161264823));
#18726=CARTESIAN_POINT('Ctrl Pts',(95.3517316765413,-2.07961226763106,-0.729985906545175));
#18727=CARTESIAN_POINT('Ctrl Pts',(95.3521187859167,-2.07724534701003,-0.736694220376826));
#18728=CARTESIAN_POINT('Ctrl Pts',(95.3529677444057,-2.07200989516625,-0.751306656927748));
#18729=CARTESIAN_POINT('Ctrl Pts',(95.3534303059727,-2.06912864128166,-0.759205742488429));
#18730=CARTESIAN_POINT('Ctrl Pts',(95.3547315688507,-2.0609409712885,-0.781259773280101));
#18731=CARTESIAN_POINT('Ctrl Pts',(95.3555758612454,-2.05553411646912,-0.79537663452365));
#18732=CARTESIAN_POINT('Ctrl Pts',(95.3613899425521,-2.01762655312087,-0.891381522397193));
#18733=CARTESIAN_POINT('Ctrl Pts',(95.3665884186582,-1.98038890814476,-0.97130573327736));
#18734=CARTESIAN_POINT('Ctrl Pts',(95.3734099528768,-1.9260764533148,-1.0716922058127));
#18735=CARTESIAN_POINT('Ctrl Pts',(95.3749724793129,-1.91327453146763,-1.09438349446007));
#18736=CARTESIAN_POINT('Ctrl Pts',(95.3767810613996,-1.89801236690273,-1.12034887393804));
#18737=CARTESIAN_POINT('Ctrl Pts',(95.3770253481034,-1.895941542512,-1.12384972820635));
#18738=CARTESIAN_POINT('Ctrl Pts',(95.3831769747213,-1.84355640400101,-1.21185312384326));
#18739=CARTESIAN_POINT('Ctrl Pts',(95.3890872447023,-1.78764899766538,-1.29290419625753));
#18740=CARTESIAN_POINT('Ctrl Pts',(95.3998383935142,-1.67370880151235,-1.43649975285407));
#18741=CARTESIAN_POINT('Ctrl Pts',(95.4047075263484,-1.61709787956617,-1.49994326042428));
#18742=CARTESIAN_POINT('Ctrl Pts',(95.4106701402952,-1.54109606968516,-1.57579860014933));
#18743=CARTESIAN_POINT('Ctrl Pts',(95.4119040966367,-1.52499172095209,-1.59138889894475));
#18744=CARTESIAN_POINT('Ctrl Pts',(95.41388687776,-1.49850746550191,-1.61625648210513));
#18745=CARTESIAN_POINT('Ctrl Pts',(95.4146422100684,-1.48827285673878,-1.62568556507322));
#18746=CARTESIAN_POINT('Ctrl Pts',(95.4160879351943,-1.46840538832137,-1.64364446702353));
#18747=CARTESIAN_POINT('Ctrl Pts',(95.416778897694,-1.45878581941757,-1.65218808288144));
#18748=CARTESIAN_POINT('Ctrl Pts',(95.4183612773613,-1.43647285419564,-1.67165852659969));
#18749=CARTESIAN_POINT('Ctrl Pts',(95.4192502146911,-1.42372853349891,-1.68252595051968));
#18750=CARTESIAN_POINT('Ctrl Pts',(95.4221187786421,-1.38193494232217,-1.71734954849029));
#18751=CARTESIAN_POINT('Ctrl Pts',(95.4240743621843,-1.35239467543153,-1.74070747581657));
#18752=CARTESIAN_POINT('Ctrl Pts',(95.4348770846008,-1.18372154576252,-1.86719278265541));
#18753=CARTESIAN_POINT('Ctrl Pts',(95.4430972445935,-1.03341718186852,-1.95439429238572));
#18754=CARTESIAN_POINT('Ctrl Pts',(95.4561059448002,-0.787724484200567,
-2.06059029987708));
#18755=CARTESIAN_POINT('Ctrl Pts',(95.4607569631639,-0.698687068520469,
-2.09245677123985));
#18756=CARTESIAN_POINT('Ctrl Pts',(95.466761642407,-0.587900479160854,-2.1242460998172));
#18757=CARTESIAN_POINT('Ctrl Pts',(95.4678579635149,-0.567831831268026,
-2.12969843300575));
#18758=CARTESIAN_POINT('Ctrl Pts',(95.4694740602982,-0.538548417489966,
-2.13721095499995));
#18759=CARTESIAN_POINT('Ctrl Pts',(95.4699816845928,-0.529392265271298,
-2.13949734448097));
#18760=CARTESIAN_POINT('Ctrl Pts',(95.4708814260211,-0.513244831564596,
-2.1434195329337));
#18761=CARTESIAN_POINT('Ctrl Pts',(95.4712721312545,-0.506259837686835,
-2.14508007462445));
#18762=CARTESIAN_POINT('Ctrl Pts',(95.4721256321703,-0.491061226771371,
-2.14861486603422));
#18763=CARTESIAN_POINT('Ctrl Pts',(95.4725891134535,-0.482845058925799,
-2.15047613686241));
#18764=CARTESIAN_POINT('Ctrl Pts',(95.4738953834714,-0.459785370881456,
-2.15556121130354));
#18765=CARTESIAN_POINT('Ctrl Pts',(95.474743829131,-0.444919174422494,-2.15867867573241));
#18766=CARTESIAN_POINT('Ctrl Pts',(95.4807576018875,-0.340222848533257,
-2.1795062501068));
#18767=CARTESIAN_POINT('Ctrl Pts',(95.4861696692407,-0.249405281304239,
-2.19175568140264));
#18768=CARTESIAN_POINT('Ctrl Pts',(95.4929575523962,-0.13623173004743,-2.19989489871128));
#18769=CARTESIAN_POINT('Ctrl Pts',(95.4942726285816,-0.114342376030421,
-2.20114117179202));
#18770=CARTESIAN_POINT('Ctrl Pts',(95.5008280132533,-0.00526513338524706,
-2.20572002255719));
#18771=CARTESIAN_POINT('Ctrl Pts',(95.5060785569923,0.0820517259273758,
-2.2041998870168));
#18772=CARTESIAN_POINT('Ctrl Pts',(95.5170771629765,0.267674385976381,-2.18992022701718));
#18773=CARTESIAN_POINT('Ctrl Pts',(95.522783604233,0.365684163414786,-2.17570203665381));
#18774=CARTESIAN_POINT('Ctrl Pts',(95.5295808734159,0.485212425378219,-2.15005312158552));
#18775=CARTESIAN_POINT('Ctrl Pts',(95.5308657246521,0.50792865020553,-2.14480023980593));
#18776=CARTESIAN_POINT('Ctrl Pts',(95.532909601277,0.544251894957292,-2.1357914073827));
#18777=CARTESIAN_POINT('Ctrl Pts',(95.5336758879201,0.55791318582489,-2.1322635744938));
#18778=CARTESIAN_POINT('Ctrl Pts',(95.5351297429573,0.583910294686016,-2.12528323457521));
#18779=CARTESIAN_POINT('Ctrl Pts',(95.5358180275369,0.596251687883568,-2.12185390489184));
#18780=CARTESIAN_POINT('Ctrl Pts',(95.5373768491492,0.624274450115005,-2.11380336009496));
#18781=CARTESIAN_POINT('Ctrl Pts',(95.5382451573113,0.639935800518757,-2.10911484392925));
#18782=CARTESIAN_POINT('Ctrl Pts',(95.5405380110859,0.681413869186917,-2.09619306152914));
#18783=CARTESIAN_POINT('Ctrl Pts',(95.5419526883277,0.707133767294113,-2.08765709130422));
#18784=CARTESIAN_POINT('Ctrl Pts',(95.5520602599066,0.891577032631412,-2.02264378667209));
#18785=CARTESIAN_POINT('Ctrl Pts',(95.5601287313344,1.04351679964959,-1.94860846897075));
#18786=CARTESIAN_POINT('Ctrl Pts',(95.5740572533467,1.2860562419468,-1.79384788958586));
#18787=CARTESIAN_POINT('Ctrl Pts',(95.5798691309457,1.38118380651887,-1.72167234543653));
#18788=CARTESIAN_POINT('Ctrl Pts',(95.586957766528,1.48156151362213,-1.63181873150593));
#18789=CARTESIAN_POINT('Ctrl Pts',(95.5877821290291,1.49301576034949,-1.62134536834477));
#18790=CARTESIAN_POINT('Ctrl Pts',(95.5890662297948,1.51049928269737,-1.60501667506057));
#18791=CARTESIAN_POINT('Ctrl Pts',(95.5895198131222,1.51660749695779,-1.59924616794208));
#18792=CARTESIAN_POINT('Ctrl Pts',(95.5903661412603,1.52787566440592,-1.58847837593784));
#18793=CARTESIAN_POINT('Ctrl Pts',(95.5907581744162,1.53304435866003,-1.58349063347602));
#18794=CARTESIAN_POINT('Ctrl Pts',(95.5916628303367,1.54485628919361,-1.57198019149917));
#18795=CARTESIAN_POINT('Ctrl Pts',(95.5921767377798,1.55148266141522,-1.5654405838714));
#18796=CARTESIAN_POINT('Ctrl Pts',(95.593839953109,1.57266889431303,-1.54426511540557));
#18797=CARTESIAN_POINT('Ctrl Pts',(95.5950009904635,1.5870642088126,-1.52946700916441));
#18798=CARTESIAN_POINT('Ctrl Pts',(95.6031589120318,1.68568228183387,-1.42519809137343));
#18799=CARTESIAN_POINT('Ctrl Pts',(95.6105559184847,1.7624960336327,-1.32902883771935));
#18800=CARTESIAN_POINT('Ctrl Pts',(95.6246488207518,1.89309256830612,-1.13415197819525));
#18801=CARTESIAN_POINT('Ctrl Pts',(95.6313274130144,1.94815103679543,-1.03673125079674));
#18802=CARTESIAN_POINT('Ctrl Pts',(95.640207748459,2.01336603397346,-0.897623315262396));
#18803=CARTESIAN_POINT('Ctrl Pts',(95.6425976823674,2.03006154496583,-0.859197791878371));
#18804=CARTESIAN_POINT('Ctrl Pts',(95.6467460481698,2.05752911794181,-0.790701044938781));
#18805=CARTESIAN_POINT('Ctrl Pts',(95.648518844407,2.06876148045784,-0.760828693654273));
#18806=CARTESIAN_POINT('Ctrl Pts',(95.6511415320845,2.08460596864497,-0.715741625604498));
#18807=CARTESIAN_POINT('Ctrl Pts',(95.6520075361149,2.08970835938994,-0.700704724144734));
#18808=CARTESIAN_POINT('Ctrl Pts',(95.6535518824247,2.09857192153973,-0.673625274668912));
#18809=CARTESIAN_POINT('Ctrl Pts',(95.6542321742847,2.10239300148169,-0.661603202148736));
#18810=CARTESIAN_POINT('Ctrl Pts',(95.6556877164406,2.11038696478498,-0.635683407487274));
#18811=CARTESIAN_POINT('Ctrl Pts',(95.6564618405965,2.11452625516245,-0.621775896664761));
#18812=CARTESIAN_POINT('Ctrl Pts',(95.6585334509355,2.12529622520616,-0.584238185542508));
#18813=CARTESIAN_POINT('Ctrl Pts',(95.6598225976398,2.13167015555374,-0.560536094943628));
#18814=CARTESIAN_POINT('Ctrl Pts',(95.6678235601166,2.16911179324852,-0.411416925225732));
#18815=CARTESIAN_POINT('Ctrl Pts',(95.6741801527703,2.18949784149983,-0.283573553024865));
#18816=CARTESIAN_POINT('Ctrl Pts',(95.6850276761911,2.20520178753177,-0.0603466277874939));
#18817=CARTESIAN_POINT('Ctrl Pts',(95.6895563009695,2.20576043389339,0.0343016631780244));
#18818=CARTESIAN_POINT('Ctrl Pts',(95.6966991527222,2.19729268525846,0.179076170279175));
#18819=CARTESIAN_POINT('Ctrl Pts',(95.6992204194252,2.19261590158227,0.229343404499276));
#18820=CARTESIAN_POINT('Ctrl Pts',(95.7028913980054,2.18354545068685,0.300316114566162));
#18821=CARTESIAN_POINT('Ctrl Pts',(95.7039848063516,2.18057284949141,0.321189189266353));
#18822=CARTESIAN_POINT('Ctrl Pts',(95.7059471268011,2.1747766844933,0.358088071407927));
#18823=CARTESIAN_POINT('Ctrl Pts',(95.7068102461365,2.17207418910339,0.37413150152327));
#18824=CARTESIAN_POINT('Ctrl Pts',(95.7081420151513,2.167679232232,0.398567449897152));
#18825=CARTESIAN_POINT('Ctrl Pts',(95.7086037700983,2.16611501767912,0.406982789752063));
#18826=CARTESIAN_POINT('Ctrl Pts',(95.7094571660707,2.16315153019367,0.422424891951736));
#18827=CARTESIAN_POINT('Ctrl Pts',(95.7098479843354,2.16176696820754,0.429454191811165));
#18828=CARTESIAN_POINT('Ctrl Pts',(95.7107478465878,2.15851638915541,0.445542985443602));
#18829=CARTESIAN_POINT('Ctrl Pts',(95.7112581412518,2.15662760200299,0.454597551789988));
#18830=CARTESIAN_POINT('Ctrl Pts',(95.7128687393648,2.15052232360286,0.482970726759335));
#18831=CARTESIAN_POINT('Ctrl Pts',(95.7139796340458,2.14610292427187,0.502244133966514));
#18832=CARTESIAN_POINT('Ctrl Pts',(95.7229895926815,2.10855033481861,0.656458953458616));
#18833=CARTESIAN_POINT('Ctrl Pts',(95.7314048307316,2.06298494827918,0.788042533456589));
#18834=CARTESIAN_POINT('Ctrl Pts',(95.7487479361909,1.94306220184258,1.05102654663725));
#18835=CARTESIAN_POINT('Ctrl Pts',(95.7576054923856,1.86698486334045,1.18090144705656));
#18836=CARTESIAN_POINT('Ctrl Pts',(95.7673861039803,1.76334942018843,1.3224423349996));
#18837=CARTESIAN_POINT('Ctrl Pts',(95.7687820044639,1.74806671521988,1.34257876541355));
#18838=CARTESIAN_POINT('Ctrl Pts',(95.7709589004507,1.72345924121324,1.37386874572588));
#18839=CARTESIAN_POINT('Ctrl Pts',(95.7717489113165,1.71436509842713,1.38520013360085));
#18840=CARTESIAN_POINT('Ctrl Pts',(95.7732228567288,1.69709168361481,1.40629227189789));
#18841=CARTESIAN_POINT('Ctrl Pts',(95.7739078042913,1.68893861664057,1.41607361929557));
#18842=CARTESIAN_POINT('Ctrl Pts',(95.7754409038375,1.67040818160355,1.43791712781092));
#18843=CARTESIAN_POINT('Ctrl Pts',(95.7762870848897,1.65998398318963,1.44993874117821));
#18844=CARTESIAN_POINT('Ctrl Pts',(95.7787680565528,1.62884817561953,1.48506988558187));
#18845=CARTESIAN_POINT('Ctrl Pts',(95.7803878099119,1.60777724573105,1.50785655730095));
#18846=CARTESIAN_POINT('Ctrl Pts',(95.7893344695021,1.4873998114667,1.63264255748545));
#18847=CARTESIAN_POINT('Ctrl Pts',(95.7962413657524,1.37887401218256,1.72528000637141));
#18848=CARTESIAN_POINT('Ctrl Pts',(95.8079801417246,1.1797677045359,1.86436744725722));
#18849=CARTESIAN_POINT('Ctrl Pts',(95.8128201104091,1.09353676705612,1.91621837215105));
#18850=CARTESIAN_POINT('Ctrl Pts',(95.8202718266607,0.961749684533358,1.98366180117435));
#18851=CARTESIAN_POINT('Ctrl Pts',(95.8227128197106,0.918737412880803,2.00394549691982));
#18852=CARTESIAN_POINT('Ctrl Pts',(95.8259065174295,0.863373693755141,2.0278967612562));
#18853=CARTESIAN_POINT('Ctrl Pts',(95.8265887372844,0.851597704004847,2.03287007561598));
#18854=CARTESIAN_POINT('Ctrl Pts',(95.8276974344113,0.832558451105272,2.04071639952598));
#18855=CARTESIAN_POINT('Ctrl Pts',(95.8281201522932,0.82532184801243,2.04365379678735));
#18856=CARTESIAN_POINT('Ctrl Pts',(95.8289420143414,0.811300404204055,2.04925859825603));
#18857=CARTESIAN_POINT('Ctrl Pts',(95.8293408653693,0.804517714741855,2.0519308930117));
#18858=CARTESIAN_POINT('Ctrl Pts',(95.8303281900514,0.787777955806871,2.05843039334748));
#18859=CARTESIAN_POINT('Ctrl Pts',(95.8309188918746,0.777806174994637,2.06221903214667));
#18860=CARTESIAN_POINT('Ctrl Pts',(95.8329892428514,0.742989191283577,2.07515881019842));
#18861=CARTESIAN_POINT('Ctrl Pts',(95.834488632611,0.718007781568828,2.0839341941399));
#18862=CARTESIAN_POINT('Ctrl Pts',(95.8442150073206,0.556976623642962,2.13726155619314));
#18863=CARTESIAN_POINT('Ctrl Pts',(95.852921678368,0.417023127279817,2.16891640321994));
#18864=CARTESIAN_POINT('Ctrl Pts',(95.8669634457191,0.18425917300624,2.19818742617519));
#18865=CARTESIAN_POINT('Ctrl Pts',(95.8723731099742,0.0928936498329579,
2.2039402670841));
#18866=CARTESIAN_POINT('Ctrl Pts',(95.8776583114079,0.000952142118494687,
2.20399984587122));
#18867=CARTESIAN_POINT('Ctrl Pts',(95.8776856739115,0.00047607047170703,
2.204));
#18868=CARTESIAN_POINT('Ctrl Pts',(95.8777130322977,9.44243789243157E-12,
2.204));
#18869=CARTESIAN_POINT('Origin',(66.9212607628943,0.,0.));
#18870=CARTESIAN_POINT('',(96.7328779004031,-1.24027783152639E-11,2.204));
#18871=CARTESIAN_POINT('',(96.6270503826334,2.66056133811156E-11,2.204));
#18872=CARTESIAN_POINT('',(66.9212607628943,-2.69912154532077E-16,2.204));
#18873=CARTESIAN_POINT('Ctrl Pts',(96.7328779004031,-1.24027783152639E-11,
2.204));
#18874=CARTESIAN_POINT('Ctrl Pts',(96.7298587062484,0.0517545618109105,
2.20400000000029));
#18875=CARTESIAN_POINT('Ctrl Pts',(96.7268830575451,0.103495927703961,2.20217705427766));
#18876=CARTESIAN_POINT('Ctrl Pts',(96.7221848298922,0.186495648980921,2.19632059943722));
#18877=CARTESIAN_POINT('Ctrl Pts',(96.720429239674,0.21781298812238,2.1934362192633));
#18878=CARTESIAN_POINT('Ctrl Pts',(96.7179163743073,0.263072049046784,2.18828882936624));
#18879=CARTESIAN_POINT('Ctrl Pts',(96.7171425675157,0.277069637214047,2.18656061725319));
#18880=CARTESIAN_POINT('Ctrl Pts',(96.7157268188338,0.302788217248647,2.18313433596879));
#18881=CARTESIAN_POINT('Ctrl Pts',(96.7150836534011,0.314513889386896,2.18147593488228));
#18882=CARTESIAN_POINT('Ctrl Pts',(96.7137618316973,0.338696114093211,2.17785672957963));
#18883=CARTESIAN_POINT('Ctrl Pts',(96.713083599525,0.351150366810158,2.17588336574876));
#18884=CARTESIAN_POINT('Ctrl Pts',(96.711563271397,0.379167539115507,2.17119725399933));
#18885=CARTESIAN_POINT('Ctrl Pts',(96.7107231352499,0.394719693527861,2.16842383302871));
#18886=CARTESIAN_POINT('Ctrl Pts',(96.7082535827562,0.440626351374217,2.15972702577093));
#18887=CARTESIAN_POINT('Ctrl Pts',(96.7066391420978,0.470888117383112,2.153331584336));
#18888=CARTESIAN_POINT('Ctrl Pts',(96.7003113553379,0.590290881787022,2.12545966350238));
#18889=CARTESIAN_POINT('Ctrl Pts',(96.6957518031178,0.678192929259821,2.09906612257732));
#18890=CARTESIAN_POINT('Ctrl Pts',(96.6867015964908,0.851930830914635,2.03484106666446));
#18891=CARTESIAN_POINT('Ctrl Pts',(96.6822229729324,0.93750659570956,1.99685893689979));
#18892=CARTESIAN_POINT('Ctrl Pts',(96.6731767779031,1.10235572269818,1.91075246792145));
#18893=CARTESIAN_POINT('Ctrl Pts',(96.6686184234022,1.18151960766259,1.86283961259836));
#18894=CARTESIAN_POINT('Ctrl Pts',(96.6627311490356,1.27427958075199,1.79840158965566));
#18895=CARTESIAN_POINT('Ctrl Pts',(96.6616493835604,1.29096063522673,1.7864650308343));
#18896=CARTESIAN_POINT('Ctrl Pts',(96.6600538392141,1.31498356875106,1.76876263951179));
#18897=CARTESIAN_POINT('Ctrl Pts',(96.6595518802614,1.32245970809196,1.76317990435572));
#18898=CARTESIAN_POINT('Ctrl Pts',(96.6586652879418,1.33551601020759,1.75330048302545));
#18899=CARTESIAN_POINT('Ctrl Pts',(96.6582820656044,1.34111135262955,1.74902428107412));
#18900=CARTESIAN_POINT('Ctrl Pts',(96.6574423249083,1.35326615873188,1.73964243244621));
#18901=CARTESIAN_POINT('Ctrl Pts',(96.6569851153289,1.35981716602655,1.73452655196312));
#18902=CARTESIAN_POINT('Ctrl Pts',(96.6557009744709,1.37803640082422,1.72013194849655));
#18903=CARTESIAN_POINT('Ctrl Pts',(96.6548686110781,1.38963944384994,1.71077188238951));
#18904=CARTESIAN_POINT('Ctrl Pts',(96.6493173880117,1.46574206377966,1.64809556865459));
#18905=CARTESIAN_POINT('Ctrl Pts',(96.6443915653548,1.52724993027945,1.59126486937166));
#18906=CARTESIAN_POINT('Ctrl Pts',(96.6374376088515,1.60819359062454,1.50745102446577));
#18907=CARTESIAN_POINT('Ctrl Pts',(96.6354670936563,1.63048349340914,1.48331343521399));
#18908=CARTESIAN_POINT('Ctrl Pts',(96.6279667872646,1.7131364560409,1.38969409152123));
#18909=CARTESIAN_POINT('Ctrl Pts',(96.6224320532924,1.76966914143734,1.31695055541269));
#18910=CARTESIAN_POINT('Ctrl Pts',(96.6115647818015,1.87357327411752,1.16442989091331));
#18911=CARTESIAN_POINT('Ctrl Pts',(96.6062444122136,1.92079611274914,1.08476700431298));
#18912=CARTESIAN_POINT('Ctrl Pts',(96.5998373135974,1.97324066745255,0.982067510776416));
#18913=CARTESIAN_POINT('Ctrl Pts',(96.5985820640037,1.98328968815008,0.961611873570815));
#18914=CARTESIAN_POINT('Ctrl Pts',(96.5965786147738,1.99895715881967,0.928428595108936));
#18915=CARTESIAN_POINT('Ctrl Pts',(96.5958235429508,2.00477534285466,0.915797584706416));
#18916=CARTESIAN_POINT('Ctrl Pts',(96.5943870091824,2.01567584981854,0.891531293400016));
#18917=CARTESIAN_POINT('Ctrl Pts',(96.5937048898292,2.02077792450716,0.879905544831762));
#18918=CARTESIAN_POINT('Ctrl Pts',(96.5921548841836,2.03219976820538,0.853255958858069));
#18919=CARTESIAN_POINT('Ctrl Pts',(96.5912892529352,2.03845395041385,0.838204712786434));
#18920=CARTESIAN_POINT('Ctrl Pts',(96.5889926972575,2.05470533783437,0.797836323920241));
#18921=CARTESIAN_POINT('Ctrl Pts',(96.5875718126063,2.06440164097361,0.772400656605027));
#18922=CARTESIAN_POINT('Ctrl Pts',(96.5775921605438,2.12983699459136,0.59070546889544));
#18923=CARTESIAN_POINT('Ctrl Pts',(96.5696359863537,2.16824727422706,0.428774070994789));
#18924=CARTESIAN_POINT('Ctrl Pts',(96.555715832866,2.20270903089398,0.143202550637772));
#18925=CARTESIAN_POINT('Ctrl Pts',(96.5497911605003,2.2072541266064,0.0213628324410037));
#18926=CARTESIAN_POINT('Ctrl Pts',(96.5425741760836,2.20101873445896,-0.115632143233154));
#18927=CARTESIAN_POINT('Ctrl Pts',(96.5417542281166,2.20015494612941,-0.131043688883808));
#18928=CARTESIAN_POINT('Ctrl Pts',(96.54047827966,2.1985755898818,-0.15476059050655));
#18929=CARTESIAN_POINT('Ctrl Pts',(96.5400283822173,2.19797464339611,-0.163073379662546));
#18930=CARTESIAN_POINT('Ctrl Pts',(96.5391899279623,2.19677393458744,-0.178467895348348));
#18931=CARTESIAN_POINT('Ctrl Pts',(96.538802081181,2.19618705246131,-0.185550358088997));
#18932=CARTESIAN_POINT('Ctrl Pts',(96.5379088132156,2.19476353542312,-0.201775391509915));
#18933=CARTESIAN_POINT('Ctrl Pts',(96.5374021550974,2.19390402140018,-0.210915679265884));
#18934=CARTESIAN_POINT('Ctrl Pts',(96.5357696590319,2.19096774919756,-0.240178134856074));
#18935=CARTESIAN_POINT('Ctrl Pts',(96.5346325734951,2.18867111050859,-0.260276632143668));
#18936=CARTESIAN_POINT('Ctrl Pts',(96.5258988237355,2.16911475275039,-0.412777635752838));
#18937=CARTESIAN_POINT('Ctrl Pts',(96.5178279836494,2.14013273103775,-0.543388703291366));
#18938=CARTESIAN_POINT('Ctrl Pts',(96.5035189610641,2.06761705366597,-0.770432986581292));
#18939=CARTESIAN_POINT('Ctrl Pts',(96.497274181195,2.02863230900659,-0.86790649589299));
#18940=CARTESIAN_POINT('Ctrl Pts',(96.487750334366,1.95656074921,-1.01642159639436));
#18941=CARTESIAN_POINT('Ctrl Pts',(96.4843422138979,1.92805685706703,-1.06950482067662));
#18942=CARTESIAN_POINT('Ctrl Pts',(96.4799031192365,1.88723268634588,-1.13858205323129));
#18943=CARTESIAN_POINT('Ctrl Pts',(96.4788047072727,1.87681886184179,-1.15566747011969));
#18944=CARTESIAN_POINT('Ctrl Pts',(96.4769894666453,1.85908921644074,-1.18388368911044));
#18945=CARTESIAN_POINT('Ctrl Pts',(96.4762679371796,1.85190271705765,-1.19509398856278));
#18946=CARTESIAN_POINT('Ctrl Pts',(96.4748593059076,1.83760027569854,-1.21696569465826));
#18947=CARTESIAN_POINT('Ctrl Pts',(96.4741719545914,1.83049206110129,-1.22763149969902));
#18948=CARTESIAN_POINT('Ctrl Pts',(96.4725209436016,1.81310797930154,-1.25322942380201));
#18949=CARTESIAN_POINT('Ctrl Pts',(96.4715608104923,1.80274007529805,-1.26809809577788));
#18950=CARTESIAN_POINT('Ctrl Pts',(96.4683742223232,1.76747742709525,-1.31736182273613));
#18951=CARTESIAN_POINT('Ctrl Pts',(96.4661788483208,1.74177176961209,-1.35116617594726));
#18952=CARTESIAN_POINT('Ctrl Pts',(96.4554881932676,1.60997993211048,-1.51446295414412));
#18953=CARTESIAN_POINT('Ctrl Pts',(96.4475477520423,1.49036363473989,-1.63231477228739));
#18954=CARTESIAN_POINT('Ctrl Pts',(96.4349001214269,1.2855960016709,-1.79260817523177));
#18955=CARTESIAN_POINT('Ctrl Pts',(96.4303323226413,1.20911321032597,-1.84505914537632));
#18956=CARTESIAN_POINT('Ctrl Pts',(96.4244334792825,1.11193485019172,-1.90306028906805));
#18957=CARTESIAN_POINT('Ctrl Pts',(96.423350653709,1.09415855698485,-1.91333597870521));
#18958=CARTESIAN_POINT('Ctrl Pts',(96.4217538268103,1.06809611167613,-1.9279195592932));
#18959=CARTESIAN_POINT('Ctrl Pts',(96.4212516721216,1.05992155539367,-1.93242578665264));
#18960=CARTESIAN_POINT('Ctrl Pts',(96.4203614126176,1.04547342448672,-1.94027106954058));
#18961=CARTESIAN_POINT('Ctrl Pts',(96.4199746868572,1.03921197453441,-1.94363190320233));
#18962=CARTESIAN_POINT('Ctrl Pts',(96.4191300348318,1.02557000091429,-1.9508694649369));
#18963=CARTESIAN_POINT('Ctrl Pts',(96.4186714376794,1.01818381162755,-1.95473456434584));
#18964=CARTESIAN_POINT('Ctrl Pts',(96.4173797509022,0.997431044739363,-1.96544469033682));
#18965=CARTESIAN_POINT('Ctrl Pts',(96.4165411310799,0.98401641919931,-1.97219501602865));
#18966=CARTESIAN_POINT('Ctrl Pts',(96.410744421575,0.891605491706431,-2.01751926707621));
#18967=CARTESIAN_POINT('Ctrl Pts',(96.4055582108929,0.8104381691074,-2.05147055941209));
#18968=CARTESIAN_POINT('Ctrl Pts',(96.3985615152765,0.699920226692501,-2.09011469096104));
#18969=CARTESIAN_POINT('Ctrl Pts',(96.3968104610436,0.672182761178849,-2.09919938336));
#18970=CARTESIAN_POINT('Ctrl Pts',(96.3894447416618,0.554902356093236,-2.13504867185127));
#18971=CARTESIAN_POINT('Ctrl Pts',(96.3838258973558,0.463880063521639,-2.15665628082435));
#18972=CARTESIAN_POINT('Ctrl Pts',(96.3729995290388,0.282476290138551,-2.18769919487842));
#18973=CARTESIAN_POINT('Ctrl Pts',(96.367794764798,0.192330452159084,-2.1974605338748));
#18974=CARTESIAN_POINT('Ctrl Pts',(96.361502920852,0.0791899529410651,-2.20269349493717));
#18975=CARTESIAN_POINT('Ctrl Pts',(96.3602546855457,0.0565342480874049,
-2.20339138926516));
#18976=CARTESIAN_POINT('Ctrl Pts',(96.3582596583508,0.0199934536269167,
-2.20395301649099));
#18977=CARTESIAN_POINT('Ctrl Pts',(96.3575060976031,0.00611379565499054,
-2.20403522453194));
#18978=CARTESIAN_POINT('Ctrl Pts',(96.3560707000286,-0.0204690278131193,
-2.20394155760186));
#18979=CARTESIAN_POINT('Ctrl Pts',(96.3553882256754,-0.0331716689551365,
-2.20378697250126));
#18980=CARTESIAN_POINT('Ctrl Pts',(96.3538350414583,-0.062221193836304,
-2.20318222583736));
#18981=CARTESIAN_POINT('Ctrl Pts',(96.3529666201739,-0.0785659273935716,
-2.20265994010033));
#18982=CARTESIAN_POINT('Ctrl Pts',(96.3506573723257,-0.122287881182493,
-2.20077553689516));
#18983=CARTESIAN_POINT('Ctrl Pts',(96.3492267672784,-0.14964845323569,-2.19908451777842));
#18984=CARTESIAN_POINT('Ctrl Pts',(96.3393693434932,-0.339835212465662,
-2.18376391691758));
#18985=CARTESIAN_POINT('Ctrl Pts',(96.3315239046375,-0.500734303607521,
-2.15257587248012));
#18986=CARTESIAN_POINT('Ctrl Pts',(96.3194567346258,-0.738832767997645,
-2.07825452945098));
#18987=CARTESIAN_POINT('Ctrl Pts',(96.3152780830522,-0.81937152232122,-2.04783894355926));
#18988=CARTESIAN_POINT('Ctrl Pts',(96.3087323218619,-0.937625363321509,
-1.99508515793927));
#18989=CARTESIAN_POINT('Ctrl Pts',(96.3064923112489,-0.976793923398442,
-1.97620324417918));
#18990=CARTESIAN_POINT('Ctrl Pts',(96.3035343874477,-1.02632970060474,-1.95049113229691));
#18991=CARTESIAN_POINT('Ctrl Pts',(96.302875212988,-1.03723524986854,-1.9447136894284));
#18992=CARTESIAN_POINT('Ctrl Pts',(96.3017976320076,-1.05483302867817,-1.9352007677892));
#18993=CARTESIAN_POINT('Ctrl Pts',(96.3013826695694,-1.06155544978605,-1.93152135722222));
#18994=CARTESIAN_POINT('Ctrl Pts',(96.3005704859288,-1.07460352443904,-1.9242910090979));
#18995=CARTESIAN_POINT('Ctrl Pts',(96.3001734938825,-1.08093105211585,-1.92074378251485));
#18996=CARTESIAN_POINT('Ctrl Pts',(96.2992782748842,-1.09509041342977,-1.91271388845832));
#18997=CARTESIAN_POINT('Ctrl Pts',(96.2987789919525,-1.10291245896627,-1.90821422664363));
#18998=CARTESIAN_POINT('Ctrl Pts',(96.2972685697199,-1.12635969329858,-1.89453378808253));
#18999=CARTESIAN_POINT('Ctrl Pts',(96.2962490116705,-1.14189913779627,-1.88520841012762));
#19000=CARTESIAN_POINT('Ctrl Pts',(96.2875501055493,-1.27225408843843,-1.80477809475657));
#19001=CARTESIAN_POINT('Ctrl Pts',(96.2793825462485,-1.38041768628292,-1.72345484399622));
#19002=CARTESIAN_POINT('Ctrl Pts',(96.2620224217044,-1.59466361771938,-1.52919355031917));
#19003=CARTESIAN_POINT('Ctrl Pts',(96.2529129148622,-1.69771174068804,-1.41392152406733));
#19004=CARTESIAN_POINT('Ctrl Pts',(96.2429294759101,-1.80246924960868,-1.26859842126896));
#19005=CARTESIAN_POINT('Ctrl Pts',(96.2415533500128,-1.81670190309005,-1.24813125014843));
#19006=CARTESIAN_POINT('Ctrl Pts',(96.2394050181618,-1.83858429092446,-1.2154958400654));
#19007=CARTESIAN_POINT('Ctrl Pts',(96.2386240650529,-1.84646717528242,-1.20348714841613));
#19008=CARTESIAN_POINT('Ctrl Pts',(96.2371659376323,-1.8610473007181,-1.18079544781625));
#19009=CARTESIAN_POINT('Ctrl Pts',(96.2364877827042,-1.86777133252527,-1.1701304216466));
#19010=CARTESIAN_POINT('Ctrl Pts',(96.2349686945983,-1.88270170864102,-1.14599263121544));
#19011=CARTESIAN_POINT('Ctrl Pts',(96.2341297072409,-1.89085571056936,-1.13248820473646));
#19012=CARTESIAN_POINT('Ctrl Pts',(96.2316669347595,-1.91450914345224,-1.09234630607763));
#19013=CARTESIAN_POINT('Ctrl Pts',(96.230057999298,-1.92959598805286,-1.06546945438629));
#19014=CARTESIAN_POINT('Ctrl Pts',(96.2208902421419,-2.01327070776364,-0.908794369701065));
#19015=CARTESIAN_POINT('Ctrl Pts',(96.2137825675048,-2.06931817481662,-0.772718120787975));
#19016=CARTESIAN_POINT('Ctrl Pts',(96.2019722323974,-2.13939872201444,-0.538614425396601));
#19017=CARTESIAN_POINT('Ctrl Pts',(96.1972664119603,-2.16113786367353,-0.443411023906599));
#19018=CARTESIAN_POINT('Ctrl Pts',(96.190770106816,-2.18144316652708,-0.316081511794287));
#19019=CARTESIAN_POINT('Ctrl Pts',(96.1891669793782,-2.18572436781954,-0.284974799212456));
#19020=CARTESIAN_POINT('Ctrl Pts',(96.1863915083369,-2.19187086812668,-0.231951235647986));
#19021=CARTESIAN_POINT('Ctrl Pts',(96.1852342482009,-2.19407530070379,-0.210078034978104));
#19022=CARTESIAN_POINT('Ctrl Pts',(96.1835475923921,-2.19677102643225,-0.178619860766554));
#19023=CARTESIAN_POINT('Ctrl Pts',(96.1830319920775,-2.19752753828242,-0.169058300116004));
#19024=CARTESIAN_POINT('Ctrl Pts',(96.1821268192902,-2.19873790515057,-0.152376273290863));
#19025=CARTESIAN_POINT('Ctrl Pts',(96.1817387926847,-2.1992196328568,-0.145258079537501));
#19026=CARTESIAN_POINT('Ctrl Pts',(96.1809018371755,-2.20017923892677,-0.12997754920019));
#19027=CARTESIAN_POINT('Ctrl Pts',(96.1804523526847,-2.20064625762887,-0.121814986954735));
#19028=CARTESIAN_POINT('Ctrl Pts',(96.1792099453642,-2.20180537330854,-0.099366339046418));
#19029=CARTESIAN_POINT('Ctrl Pts',(96.1784121188526,-2.2024038259397,-0.0850760645741195));
#19030=CARTESIAN_POINT('Ctrl Pts',(96.1739629677143,-2.20494451851432,-0.00600443790338455));
#19031=CARTESIAN_POINT('Ctrl Pts',(96.1701874461072,-2.20416748301859,0.0588277015573228));
#19032=CARTESIAN_POINT('Ctrl Pts',(96.1586782428498,-2.19327258113049,0.25291414937311));
#19033=CARTESIAN_POINT('Ctrl Pts',(96.1507986496064,-2.17461207464266,0.381410593607804));
#19034=CARTESIAN_POINT('Ctrl Pts',(96.1389275963061,-2.12848995926026,0.576319375782066));
#19035=CARTESIAN_POINT('Ctrl Pts',(96.1347994120104,-2.10890976081063,0.644293785467398));
#19036=CARTESIAN_POINT('Ctrl Pts',(96.1281014541804,-2.0710249581277,0.755415431289594));
#19037=CARTESIAN_POINT('Ctrl Pts',(96.1254796049882,-2.05455361061072,0.799128760987092));
#19038=CARTESIAN_POINT('Ctrl Pts',(96.1218960358074,-2.0297241599183,0.859167905062853));
#19039=CARTESIAN_POINT('Ctrl Pts',(96.1208956258372,-2.02253376811235,0.875960524036639));
#19040=CARTESIAN_POINT('Ctrl Pts',(96.1191969427666,-2.00988157748188,0.904522141607754));
#19041=CARTESIAN_POINT('Ctrl Pts',(96.1184951864292,-2.00452319096668,0.916335662904017));
#19042=CARTESIAN_POINT('Ctrl Pts',(96.1171645534972,-1.99411260818709,0.938759277380746));
#19043=CARTESIAN_POINT('Ctrl Pts',(96.116535057678,-1.98907925715543,0.949377580905073));
#19044=CARTESIAN_POINT('Ctrl Pts',(96.1149108389728,-1.97581237671403,0.976796541353063));
#19045=CARTESIAN_POINT('Ctrl Pts',(96.1139206487809,-1.96744932289345,0.993533704451851));
#19046=CARTESIAN_POINT('Ctrl Pts',(96.1105119383601,-1.93771430084698,1.05119487221928));
#19047=CARTESIAN_POINT('Ctrl Pts',(96.1081309597193,-1.91526976558125,1.09155370110274));
#19048=CARTESIAN_POINT('Ctrl Pts',(96.0974763412222,-1.80754904164396,1.27168565626526));
#19049=CARTESIAN_POINT('Ctrl Pts',(96.0897122521212,-1.70813519191704,1.40238852894118));
#19050=CARTESIAN_POINT('Ctrl Pts',(96.0772977374628,-1.53208161842689,1.58704068838235));
#19051=CARTESIAN_POINT('Ctrl Pts',(96.0727871653501,-1.46495250369248,1.64920688511033));
#19052=CARTESIAN_POINT('Ctrl Pts',(96.0669584126072,-1.37836034115307,1.71992883688432));
#19053=CARTESIAN_POINT('Ctrl Pts',(96.0658820361031,-1.36237717049087,1.73261675528396));
#19054=CARTESIAN_POINT('Ctrl Pts',(96.0642930129819,-1.33884798798936,1.75076805165262));
#19055=CARTESIAN_POINT('Ctrl Pts',(96.063792050911,-1.33143943644156,1.75640875834419));
#19056=CARTESIAN_POINT('Ctrl Pts',(96.062903092883,-1.31831572276943,1.76627011798733));
#19057=CARTESIAN_POINT('Ctrl Pts',(96.0625164611658,-1.3126155828012,1.77051032329445));
#19058=CARTESIAN_POINT('Ctrl Pts',(96.0616710315912,-1.30016964150332,1.77967543635046));
#19059=CARTESIAN_POINT('Ctrl Pts',(96.0612115518424,-1.29341641468204,1.78458951273183));
#19060=CARTESIAN_POINT('Ctrl Pts',(96.0599150569335,-1.27438604106841,1.79827245982117));
#19061=CARTESIAN_POINT('Ctrl Pts',(96.059072448671,-1.26204677432791,1.80695366161149));
#19062=CARTESIAN_POINT('Ctrl Pts',(96.0530872532332,-1.17451705150402,1.8672006624702));
#19063=CARTESIAN_POINT('Ctrl Pts',(96.0476995364777,-1.09628570846837,1.91417950182016));
#19064=CARTESIAN_POINT('Ctrl Pts',(96.0406855852496,-0.992209795841663,
1.96820150625176));
#19065=CARTESIAN_POINT('Ctrl Pts',(96.0391190826225,-0.968828842654001,
1.97981516871026));
#19066=CARTESIAN_POINT('Ctrl Pts',(96.0318024193023,-0.85878304360612,2.0320602397704));
#19067=CARTESIAN_POINT('Ctrl Pts',(96.0260484077454,-0.769732212170165,
2.06743590041368));
#19068=CARTESIAN_POINT('Ctrl Pts',(96.0169783399809,-0.622860145118887,
2.11497069620432));
#19069=CARTESIAN_POINT('Ctrl Pts',(96.0135832293551,-0.566358424110971,
2.13079674148879));
#19070=CARTESIAN_POINT('Ctrl Pts',(96.0079328538014,-0.469476629841306,
2.15380642984758));
#19071=CARTESIAN_POINT('Ctrl Pts',(96.0056442138879,-0.429406823009307,
2.16215183050514));
#19072=CARTESIAN_POINT('Ctrl Pts',(96.0024339138942,-0.372021230694282,
2.17244520913536));
#19073=CARTESIAN_POINT('Ctrl Pts',(96.0014834649776,-0.354880547292618,
2.17531096727852));
#19074=CARTESIAN_POINT('Ctrl Pts',(95.9998432633233,-0.325043132595704,
2.17993743070849));
#19075=CARTESIAN_POINT('Ctrl Pts',(95.9991506125998,-0.312361790341013,
2.18179063190975));
#19076=CARTESIAN_POINT('Ctrl Pts',(95.9977314513991,-0.286215649674768,
2.1853788890441));
#19077=CARTESIAN_POINT('Ctrl Pts',(95.9970053974418,-0.272749519469492,
2.1871003629818));
#19078=CARTESIAN_POINT('Ctrl Pts',(95.9951530702239,-0.238171515371894,
2.19119639507796));
#19079=CARTESIAN_POINT('Ctrl Pts',(95.9940325028907,-0.217039406713831,
2.19339035519573));
#19080=CARTESIAN_POINT('Ctrl Pts',(95.9895002557444,-0.13075063062194,2.20108965406977));
#19081=CARTESIAN_POINT('Ctrl Pts',(95.9861693214704,-0.065393673492086,
2.20399999999966));
#19082=CARTESIAN_POINT('Ctrl Pts',(95.9829026914895,-1.13898760397551E-11,
2.204));
#19083=CARTESIAN_POINT('Ctrl Pts',(95.8777130322977,9.44243789243157E-12,
2.204));
#19084=CARTESIAN_POINT('Ctrl Pts',(95.8808140072998,-0.0539608801586369,
2.204));
#19085=CARTESIAN_POINT('Ctrl Pts',(95.8838604928531,-0.107906633747905,
2.20201831932735));
#19086=CARTESIAN_POINT('Ctrl Pts',(95.8879545246214,-0.181710970242176,
2.19658793759466));
#19087=CARTESIAN_POINT('Ctrl Pts',(95.889054454545,-0.201672495502803,2.19484525338729));
#19088=CARTESIAN_POINT('Ctrl Pts',(95.8908034985033,-0.233620308559798,
2.19161660005351));
#19089=CARTESIAN_POINT('Ctrl Pts',(95.8914580149408,-0.24562264019355,2.19030392798998));
#19090=CARTESIAN_POINT('Ctrl Pts',(95.8928075722312,-0.270464880329532,
2.18738021103148));
#19091=CARTESIAN_POINT('Ctrl Pts',(95.8935021254901,-0.283302625147236,
2.18575457715834));
#19092=CARTESIAN_POINT('Ctrl Pts',(95.8951287693371,-0.313487137988951,
2.18166193122109));
#19093=CARTESIAN_POINT('Ctrl Pts',(95.8960578569719,-0.330820409300836,
2.17910092663289));
#19094=CARTESIAN_POINT('Ctrl Pts',(95.8991486766197,-0.388770164135528,
2.16983140778018));
#19095=CARTESIAN_POINT('Ctrl Pts',(95.9012810906271,-0.429230043733431,
2.16219158011915));
#19096=CARTESIAN_POINT('Ctrl Pts',(95.9063945699805,-0.527092850754496,
2.14085713156891));
#19097=CARTESIAN_POINT('Ctrl Pts',(95.9093407535116,-0.584206248039353,
2.12598207920902));
#19098=CARTESIAN_POINT('Ctrl Pts',(95.9169361773389,-0.731795172127066,
2.08114503946293));
#19099=CARTESIAN_POINT('Ctrl Pts',(95.9215081523608,-0.821044567312776,
2.04757785988123));
#19100=CARTESIAN_POINT('Ctrl Pts',(95.9274997625985,-0.933767217458664,
1.99662320497921));
#19101=CARTESIAN_POINT('Ctrl Pts',(95.9288813308404,-0.959462567590678,
1.9844034331603));
#19102=CARTESIAN_POINT('Ctrl Pts',(95.9345948085902,-1.06404834285758,1.93215993199128));
#19103=CARTESIAN_POINT('Ctrl Pts',(95.9389961067053,-1.14072385338066,1.88790542542031));
#19104=CARTESIAN_POINT('Ctrl Pts',(95.9444480208715,-1.22714701287942,1.83083450786026));
#19105=CARTESIAN_POINT('Ctrl Pts',(95.9452515965109,-1.23968244628205,1.82236993876386));
#19106=CARTESIAN_POINT('Ctrl Pts',(95.9465148437435,-1.25905057064349,1.80899927914952));
#19107=CARTESIAN_POINT('Ctrl Pts',(95.9469688030385,-1.26594420300091,1.80418180944501));
#19108=CARTESIAN_POINT('Ctrl Pts',(95.9478117333102,-1.27861751833705,1.79521693569682));
#19109=CARTESIAN_POINT('Ctrl Pts',(95.9481999495739,-1.28440489231027,1.79108086708296));
#19110=CARTESIAN_POINT('Ctrl Pts',(95.9491066100489,-1.29780781172753,1.78140382318188));
#19111=CARTESIAN_POINT('Ctrl Pts',(95.9496264523477,-1.30540794408094,1.77584199474724));
#19112=CARTESIAN_POINT('Ctrl Pts',(95.9512981391637,-1.3295888015866,1.75790717326275));
#19113=CARTESIAN_POINT('Ctrl Pts',(95.9524617033262,-1.34603059275926,1.74534970458874));
#19114=CARTESIAN_POINT('Ctrl Pts',(95.9589470349264,-1.43571332049494,1.67483330589692));
#19115=CARTESIAN_POINT('Ctrl Pts',(95.9644994519691,-1.50538450979502,1.61249929258205));
#19116=CARTESIAN_POINT('Ctrl Pts',(95.9802807150614,-1.69001477289618,1.42488983596014));
#19117=CARTESIAN_POINT('Ctrl Pts',(95.9905170917334,-1.794771358605,1.29045441324676));
#19118=CARTESIAN_POINT('Ctrl Pts',(96.0024215117585,-1.90379577757042,1.11120257047076));
#19119=CARTESIAN_POINT('Ctrl Pts',(96.0046548435043,-1.92361006205016,1.07653803296291));
#19120=CARTESIAN_POINT('Ctrl Pts',(96.0077380873227,-1.95004753997535,1.0272232528158));
#19121=CARTESIAN_POINT('Ctrl Pts',(96.0086160212378,-1.95746804891239,1.01301129113437));
#19122=CARTESIAN_POINT('Ctrl Pts',(96.0101361766362,-1.97012612970443,0.988109652339457));
#19123=CARTESIAN_POINT('Ctrl Pts',(96.0107808261438,-1.97543333240648,0.977456295186827));
#19124=CARTESIAN_POINT('Ctrl Pts',(96.0121272015841,-1.98638815493918,0.955012558954213));
#19125=CARTESIAN_POINT('Ctrl Pts',(96.0128282786494,-1.99201770681454,0.943213844126139));
#19126=CARTESIAN_POINT('Ctrl Pts',(96.0145014510036,-2.00526991886247,0.914791222837917));
#19127=CARTESIAN_POINT('Ctrl Pts',(96.0154700332366,-2.01279136540406,0.898121024830673));
#19128=CARTESIAN_POINT('Ctrl Pts',(96.0188564699912,-2.03854251155913,0.839098513972825));
#19129=CARTESIAN_POINT('Ctrl Pts',(96.0212364979097,-2.05565049197974,0.796268377548354));
#19130=CARTESIAN_POINT('Ctrl Pts',(96.0270965374719,-2.09505313372218,0.687867002270776));
#19131=CARTESIAN_POINT('Ctrl Pts',(96.0305255265622,-2.11562543969606,0.621722218277033));
#19132=CARTESIAN_POINT('Ctrl Pts',(96.040354402202,-2.16623990399721,0.427094185954962));
#19133=CARTESIAN_POINT('Ctrl Pts',(96.0466034293222,-2.18790697071944,0.296757947577396));
#19134=CARTESIAN_POINT('Ctrl Pts',(96.0563473765552,-2.20264994410874,0.100705790308834));
#19135=CARTESIAN_POINT('Ctrl Pts',(96.0596238376294,-2.20465730361557,0.0359615739420522));
#19136=CARTESIAN_POINT('Ctrl Pts',(96.0637915706463,-2.20362567794578,-0.0430584218821372));
#19137=CARTESIAN_POINT('Ctrl Pts',(96.0645517356219,-2.20330023253847,-0.0573430045539922));
#19138=CARTESIAN_POINT('Ctrl Pts',(96.0657609964939,-2.20256874633792,-0.0798405720206565));
#19139=CARTESIAN_POINT('Ctrl Pts',(96.0662051346934,-2.20225558529642,-0.0880564128882801));
#19140=CARTESIAN_POINT('Ctrl Pts',(96.0670440285627,-2.20158120712884,-0.103480825864513));
#19141=CARTESIAN_POINT('Ctrl Pts',(96.0674382057513,-2.20123054218426,-0.110689600753901));
#19142=CARTESIAN_POINT('Ctrl Pts',(96.0683705511707,-2.20032190418409,-0.127651698556929));
#19143=CARTESIAN_POINT('Ctrl Pts',(96.0689103133956,-2.1997344827473,-0.137403188475828));
#19144=CARTESIAN_POINT('Ctrl Pts',(96.0707145129141,-2.19756761016867,-0.169785945114205));
#19145=CARTESIAN_POINT('Ctrl Pts',(96.0719933146377,-2.19570361417405,-0.192396011186734));
#19146=CARTESIAN_POINT('Ctrl Pts',(96.0751494655941,-2.19030407636597,-0.247490715104332));
#19147=CARTESIAN_POINT('Ctrl Pts',(96.0770420107452,-2.18639452925789,-0.27993280355363));
#19148=CARTESIAN_POINT('Ctrl Pts',(96.0850848020483,-2.16693521363938,-0.41588904052543));
#19149=CARTESIAN_POINT('Ctrl Pts',(96.0914102969468,-2.14474315292751,-0.518312139079507));
#19150=CARTESIAN_POINT('Ctrl Pts',(96.1058952413664,-2.07694456183987,-0.750092911015594));
#19151=CARTESIAN_POINT('Ctrl Pts',(96.1139762899925,-2.02637978732648,-0.877572031132577));
#19152=CARTESIAN_POINT('Ctrl Pts',(96.1234137563986,-1.95020209235962,-1.02727574259194));
#19153=CARTESIAN_POINT('Ctrl Pts',(96.1251416375877,-1.93550865355848,-1.05469902996348));
#19154=CARTESIAN_POINT('Ctrl Pts',(96.1277232300061,-1.91242170602501,-1.09567918420449));
#19155=CARTESIAN_POINT('Ctrl Pts',(96.1285919526992,-1.90445403989741,-1.10947036241378));
#19156=CARTESIAN_POINT('Ctrl Pts',(96.130145556035,-1.8898478100494,-1.13413113168745));
#19157=CARTESIAN_POINT('Ctrl Pts',(96.1308323533897,-1.8832632545767,-1.14503174299403));
#19158=CARTESIAN_POINT('Ctrl Pts',(96.1322947674607,-1.86897053793888,-1.1682362367599));
#19159=CARTESIAN_POINT('Ctrl Pts',(96.1330693173745,-1.86123450754118,-1.18052229893341));
#19160=CARTESIAN_POINT('Ctrl Pts',(96.1351776295511,-1.83972582079231,-1.21394451122998));
#19161=CARTESIAN_POINT('Ctrl Pts',(96.1365023330773,-1.82571058560372,-1.23492238562563));
#19162=CARTESIAN_POINT('Ctrl Pts',(96.1456196927004,-1.72584096036568,-1.37898866864711));
#19163=CARTESIAN_POINT('Ctrl Pts',(96.1529182045005,-1.62797045813742,-1.49326985766682));
#19164=CARTESIAN_POINT('Ctrl Pts',(96.1668973019706,-1.41845653199072,-1.69261576069878));
#19165=CARTESIAN_POINT('Ctrl Pts',(96.1735656384931,-1.30883669950046,-1.77873683153962));
#19166=CARTESIAN_POINT('Ctrl Pts',(96.1818558632557,-1.17522285060526,-1.86463346195436));
#19167=CARTESIAN_POINT('Ctrl Pts',(96.1828992905372,-1.15845373320334,-1.87509775490868));
#19168=CARTESIAN_POINT('Ctrl Pts',(96.1844512889781,-1.13363570433075,-1.89012476270686));
#19169=CARTESIAN_POINT('Ctrl Pts',(96.1849490231848,-1.12569474982163,-1.89486486397816));
#19170=CARTESIAN_POINT('Ctrl Pts',(96.185838088848,-1.11154951239531,-1.9031881176885));
#19171=CARTESIAN_POINT('Ctrl Pts',(96.1862281328318,-1.105357270884,-1.90679118719994));
#19172=CARTESIAN_POINT('Ctrl Pts',(96.187088608182,-1.09172733147969,-1.91463331154296));
#19173=CARTESIAN_POINT('Ctrl Pts',(96.1875598216945,-1.08428256070421,-1.91885919427631));
#19174=CARTESIAN_POINT('Ctrl Pts',(96.1889344326019,-1.0626135974916,-1.93099280220957));
#19175=CARTESIAN_POINT('Ctrl Pts',(96.1898445889073,-1.04832649274231,-1.93878631944902));
#19176=CARTESIAN_POINT('Ctrl Pts',(96.1919531741744,-1.01532802360984,-1.95631538046725));
#19177=CARTESIAN_POINT('Ctrl Pts',(96.1931570634248,-0.996560749644345,
-1.9659418801496));
#19178=CARTESIAN_POINT('Ctrl Pts',(96.197281655568,-0.932396365078903,-1.99769957127598));
#19179=CARTESIAN_POINT('Ctrl Pts',(96.2002537592485,-0.88637950854176,-2.0185384285643));
#19180=CARTESIAN_POINT('Ctrl Pts',(96.2088773582891,-0.752298370335672,
-2.07378814837831));
#19181=CARTESIAN_POINT('Ctrl Pts',(96.214593284168,-0.662680984395197,-2.1041397484341));
#19182=CARTESIAN_POINT('Ctrl Pts',(96.2279600237636,-0.446629300034757,
-2.16213449407633));
#19183=CARTESIAN_POINT('Ctrl Pts',(96.2355147290957,-0.319149454574453,
-2.18459506137907));
#19184=CARTESIAN_POINT('Ctrl Pts',(96.2440819885446,-0.165969212274163,
-2.19787910195878));
#19185=CARTESIAN_POINT('Ctrl Pts',(96.2454368808827,-0.141484277738279,
-2.19959100611417));
#19186=CARTESIAN_POINT('Ctrl Pts',(96.2475724663737,-0.102485621618808,
-2.20166374280065));
#19187=CARTESIAN_POINT('Ctrl Pts',(96.2483614130916,-0.087988623317635,
-2.2022907517718));
#19188=CARTESIAN_POINT('Ctrl Pts',(96.2498278436583,-0.0608789692863493,
-2.20319515052269));
#19189=CARTESIAN_POINT('Ctrl Pts',(96.2505063936855,-0.0482681430775895,
-2.20350750299152));
#19190=CARTESIAN_POINT('Ctrl Pts',(96.2520314430948,-0.0197791283163416,
-2.20396844350308));
#19191=CARTESIAN_POINT('Ctrl Pts',(96.2528759301563,-0.00390052936315621,
-2.20405374653897));
#19192=CARTESIAN_POINT('Ctrl Pts',(96.2554017270825,0.0438860806456116,
-2.20379404083033));
#19193=CARTESIAN_POINT('Ctrl Pts',(96.2570668024269,0.0757877150087699,
-2.20292771566959));
#19194=CARTESIAN_POINT('Ctrl Pts',(96.2608724208335,0.149494780580092,-2.19932298932911));
#19195=CARTESIAN_POINT('Ctrl Pts',(96.2629980147041,0.191263700756831,-2.196084870073));
#19196=CARTESIAN_POINT('Ctrl Pts',(96.2706937728745,0.344021171097496,-2.17985070030595));
#19197=CARTESIAN_POINT('Ctrl Pts',(96.2760771354235,0.45407090513955,-2.15961125823417));
#19198=CARTESIAN_POINT('Ctrl Pts',(96.2874200957706,0.680940333597782,-2.09977108078821));
#19199=CARTESIAN_POINT('Ctrl Pts',(96.2933659224868,0.79692616242497,-2.05854818734973));
#19200=CARTESIAN_POINT('Ctrl Pts',(96.3008444195426,0.927665345717941,-1.99936968991775));
#19201=CARTESIAN_POINT('Ctrl Pts',(96.3019329185878,0.946350665226227,-1.99059350658646));
#19202=CARTESIAN_POINT('Ctrl Pts',(96.3035342081346,0.973279495494193,-1.97748064379802));
#19203=CARTESIAN_POINT('Ctrl Pts',(96.3040349804591,0.981623649670132,-1.97335188880081));
#19204=CARTESIAN_POINT('Ctrl Pts',(96.3049279156702,0.996358903495227,-1.96594418301159));
#19205=CARTESIAN_POINT('Ctrl Pts',(96.3053187585022,1.00276048425597,-1.96268668031572));
#19206=CARTESIAN_POINT('Ctrl Pts',(96.306171202624,1.01661674971638,-1.9555503053585));
#19207=CARTESIAN_POINT('Ctrl Pts',(96.306633474237,1.02406510020186,-1.95166013392113));
#19208=CARTESIAN_POINT('Ctrl Pts',(96.3079567966919,1.04520746756161,-1.94046341411549));
#19209=CARTESIAN_POINT('Ctrl Pts',(96.3088238816187,1.05884653178706,-1.93305481195917));
#19210=CARTESIAN_POINT('Ctrl Pts',(96.3164216791809,1.17663613228743,-1.86745208267261));
#19211=CARTESIAN_POINT('Ctrl Pts',(96.3235678866878,1.27597173501087,-1.8010388410879));
#19212=CARTESIAN_POINT('Ctrl Pts',(96.3408459085113,1.50134185530338,-1.622322120633));
#19213=CARTESIAN_POINT('Ctrl Pts',(96.3509031747188,1.62085104389143,-1.50293569976867));
#19214=CARTESIAN_POINT('Ctrl Pts',(96.3618694702046,1.74247164399541,-1.3498678633229));
#19215=CARTESIAN_POINT('Ctrl Pts',(96.3633747294411,1.75894098768131,-1.32833631761434));
#19216=CARTESIAN_POINT('Ctrl Pts',(96.365763067906,1.78470144709975,-1.29333833903934));
#19217=CARTESIAN_POINT('Ctrl Pts',(96.366655938807,1.79424675237807,-1.28006325094539));
#19218=CARTESIAN_POINT('Ctrl Pts',(96.3682381492486,1.81100516791609,-1.25620076002369));
#19219=CARTESIAN_POINT('Ctrl Pts',(96.368929654712,1.81827528148879,-1.24565447781577));
#19220=CARTESIAN_POINT('Ctrl Pts',(96.3703754492904,1.83335856899735,-1.22336069177645));
#19221=CARTESIAN_POINT('Ctrl Pts',(96.3711289628327,1.84115173726136,-1.21160031270838));
#19222=CARTESIAN_POINT('Ctrl Pts',(96.3731163048136,1.86151927031364,-1.18021407001997));
#19223=CARTESIAN_POINT('Ctrl Pts',(96.3743427933663,1.87389632399892,-1.16046191943846));
#19224=CARTESIAN_POINT('Ctrl Pts',(96.3807118271914,1.93709054953012,-1.05596396247197));
#19225=CARTESIAN_POINT('Ctrl Pts',(96.3856558484739,1.98248181068108,-0.968064264965195));
#19226=CARTESIAN_POINT('Ctrl Pts',(96.3947783354814,2.05660914507512,-0.79725137336613));
#19227=CARTESIAN_POINT('Ctrl Pts',(96.3989726564833,2.08659704433845,-0.715097128535994));
#19228=CARTESIAN_POINT('Ctrl Pts',(96.4042827625629,2.11798245901127,-0.610129700973389));
#19229=CARTESIAN_POINT('Ctrl Pts',(96.4053603115707,2.12401514866286,-0.58878483374268));
#19230=CARTESIAN_POINT('Ctrl Pts',(96.4108993952927,2.15322794816694,-0.479126040137549));
#19231=CARTESIAN_POINT('Ctrl Pts',(96.4154334085284,2.1712239630383,-0.389532450254598));
#19232=CARTESIAN_POINT('Ctrl Pts',(96.4210374799336,2.1856724516899,-0.284046696415114));
#19233=CARTESIAN_POINT('Ctrl Pts',(96.4218441409211,2.18757755379661,-0.268981435426561));
#19234=CARTESIAN_POINT('Ctrl Pts',(96.4231112213859,2.19029715312867,-0.245530722723418));
#19235=CARTESIAN_POINT('Ctrl Pts',(96.4235658731679,2.1912195330178,-0.237157981412252));
#19236=CARTESIAN_POINT('Ctrl Pts',(96.4244130951769,2.19283919325712,-0.221638955970571));
#19237=CARTESIAN_POINT('Ctrl Pts',(96.4248049390325,2.19354957510567,-0.214494314918458));
#19238=CARTESIAN_POINT('Ctrl Pts',(96.4257164324376,2.19511300854282,-0.197949414526301));
#19239=CARTESIAN_POINT('Ctrl Pts',(96.4262374581256,2.19594059506856,-0.188547042465269));
#19240=CARTESIAN_POINT('Ctrl Pts',(96.4279168218778,2.19839865825663,-0.158404964924212));
#19241=CARTESIAN_POINT('Ctrl Pts',(96.4290870254262,2.19979584702298,-0.137647959640263));
#19242=CARTESIAN_POINT('Ctrl Pts',(96.4356458951889,2.20591318850858,-0.0224510290842082));
#19243=CARTESIAN_POINT('Ctrl Pts',(96.4412705508507,2.20484526854382,0.0721905304386301));
#19244=CARTESIAN_POINT('Ctrl Pts',(96.4573366679125,2.18461053880717,0.3393380691337));
#19245=CARTESIAN_POINT('Ctrl Pts',(96.4677768184736,2.15116111459607,0.51009491960279));
#19246=CARTESIAN_POINT('Ctrl Pts',(96.4796737715376,2.08671260616069,0.710360818463461));
#19247=CARTESIAN_POINT('Ctrl Pts',(96.4817362991761,2.07450677878628,0.745254218678266));
#19248=CARTESIAN_POINT('Ctrl Pts',(96.4846993030599,2.05545316494838,0.795621454311846));
#19249=CARTESIAN_POINT('Ctrl Pts',(96.4856224584723,2.04929625877823,0.811348308700729));
#19250=CARTESIAN_POINT('Ctrl Pts',(96.4872393375641,2.03812348585534,0.838948587555738));
#19251=CARTESIAN_POINT('Ctrl Pts',(96.4879355638596,2.03318315266614,0.850851546235838));
#19252=CARTESIAN_POINT('Ctrl Pts',(96.4893729656495,2.02271547909453,0.875459904383508));
#19253=CARTESIAN_POINT('Ctrl Pts',(96.4901135593119,2.01717215135409,0.888157912412327));
#19254=CARTESIAN_POINT('Ctrl Pts',(96.4920265722969,2.00246491876485,0.920999428082396));
#19255=CARTESIAN_POINT('Ctrl Pts',(96.4931926345052,1.99311660638524,0.941058944934252));
#19256=CARTESIAN_POINT('Ctrl Pts',(96.4985922015641,1.94805562063296,1.03406555191182));
#19257=CARTESIAN_POINT('Ctrl Pts',(96.5026956439856,1.90862895577387,1.10514684782467));
#19258=CARTESIAN_POINT('Ctrl Pts',(96.5156576513813,1.76903981148894,1.32695949385321));
#19259=CARTESIAN_POINT('Ctrl Pts',(96.5240772148112,1.65425205797801,1.46757065035644));
#19260=CARTESIAN_POINT('Ctrl Pts',(96.5354440708961,1.4914669418121,1.62330492191023));
#19261=CARTESIAN_POINT('Ctrl Pts',(96.5377303964993,1.45842186891647,1.65305706402045));
#19262=CARTESIAN_POINT('Ctrl Pts',(96.5407682284135,1.41462075458636,1.69015733325009));
#19263=CARTESIAN_POINT('Ctrl Pts',(96.5414591065936,1.40466612875451,1.69843950172202));
#19264=CARTESIAN_POINT('Ctrl Pts',(96.5425784908134,1.38856340245142,1.71159844806368));
#19265=CARTESIAN_POINT('Ctrl Pts',(96.5430031055143,1.38246108896063,1.71653106689915));
#19266=CARTESIAN_POINT('Ctrl Pts',(96.543830360968,1.37058773378974,1.72602414988892));
#19267=CARTESIAN_POINT('Ctrl Pts',(96.5442327249973,1.364820018347,1.73058845884856));
#19268=CARTESIAN_POINT('Ctrl Pts',(96.5452212693439,1.35066447658931,1.7416757383585));
#19269=CARTESIAN_POINT('Ctrl Pts',(96.5458096101251,1.34225216010275,1.74816705014371));
#19270=CARTESIAN_POINT('Ctrl Pts',(96.5479704986416,1.31138541587505,1.77163104600969));
#19271=CARTESIAN_POINT('Ctrl Pts',(96.5495658966372,1.28865420153447,1.78823333785824));
#19272=CARTESIAN_POINT('Ctrl Pts',(96.5537087194223,1.22958715755054,1.82966328312686));
#19273=CARTESIAN_POINT('Ctrl Pts',(96.556285058024,1.19281498195989,1.85384582252322));
#19274=CARTESIAN_POINT('Ctrl Pts',(96.5655614583133,1.05936529084845,1.93599174657397));
#19275=CARTESIAN_POINT('Ctrl Pts',(96.5723961032028,0.958995110198635,1.98762356678948));
#19276=CARTESIAN_POINT('Ctrl Pts',(96.5847689810228,0.767726715869882,2.06813971887748));
#19277=CARTESIAN_POINT('Ctrl Pts',(96.5903298254906,0.678047697994684,2.09925241391017));
#19278=CARTESIAN_POINT('Ctrl Pts',(96.5980266060704,0.547395846853923,2.13532922936114));
#19279=CARTESIAN_POINT('Ctrl Pts',(96.6003053630503,0.507862131127759,2.14507563875295));
#19280=CARTESIAN_POINT('Ctrl Pts',(96.6034400782898,0.452286697971418,2.15715412658319));
#19281=CARTESIAN_POINT('Ctrl Pts',(96.6043252964105,0.436456653689497,2.16041264394223));
#19282=CARTESIAN_POINT('Ctrl Pts',(96.6058544683153,0.408878107883364,2.16577401668957));
#19283=CARTESIAN_POINT('Ctrl Pts',(96.6065009223488,0.397145862726018,2.16795608120854));
#19284=CARTESIAN_POINT('Ctrl Pts',(96.6078476670213,0.372553150141126,2.17232370969069));
#19285=CARTESIAN_POINT('Ctrl Pts',(96.6085473404807,0.359689810180622,2.17449060699851));
#19286=CARTESIAN_POINT('Ctrl Pts',(96.6099331970021,0.334042858564615,2.17857716164128));
#19287=CARTESIAN_POINT('Ctrl Pts',(96.6106194172299,0.321260097474045,2.18049880531059));
#19288=CARTESIAN_POINT('Ctrl Pts',(96.6122266909798,0.29113005146125,2.18475757354844));
#19289=CARTESIAN_POINT('Ctrl Pts',(96.6131448003547,0.273770243327787,2.18700074047738));
#19290=CARTESIAN_POINT('Ctrl Pts',(96.6185207744709,0.171291457976957,2.19900330011054));
#19291=CARTESIAN_POINT('Ctrl Pts',(96.6228297409556,0.0856854896088731,
2.20399999999897));
#19292=CARTESIAN_POINT('Ctrl Pts',(96.6270503826334,2.66056133811156E-11,
2.204));
#19293=CARTESIAN_POINT('Origin',(66.9212607628943,0.,0.));
#19294=CARTESIAN_POINT('',(97.4861833980632,-2.69730385036004E-13,2.204));
#19295=CARTESIAN_POINT('',(97.3739726165667,2.84962952926334E-13,2.204));
#19296=CARTESIAN_POINT('',(66.9212607628943,-2.69912154532077E-16,2.204));
#19297=CARTESIAN_POINT('',(96.7329774739213,-0.00170103368875552,2.20399915589494));
#19298=CARTESIAN_POINT('Ctrl Pts',(97.4861833980632,7.30595079061364E-14,
2.204));
#19299=CARTESIAN_POINT('Ctrl Pts',(97.4843902495947,0.0314723260755802,
2.204));
#19300=CARTESIAN_POINT('Ctrl Pts',(97.4825693510585,0.0629397455639223,
2.20332587853465));
#19301=CARTESIAN_POINT('Ctrl Pts',(97.4749354119193,0.193342401425828,2.19773659949954));
#19302=CARTESIAN_POINT('Ctrl Pts',(97.4689606176528,0.29190213610691,2.18682858080225));
#19303=CARTESIAN_POINT('Ctrl Pts',(97.454325322464,0.531846115290877,2.14375915178902));
#19304=CARTESIAN_POINT('Ctrl Pts',(97.4457527927398,0.67145579133593,2.10421529188373));
#19305=CARTESIAN_POINT('Ctrl Pts',(97.4358871645072,0.834927485476195,2.03996695847093));
#19306=CARTESIAN_POINT('Ctrl Pts',(97.43417271346,0.863420783249822,2.02807144476291));
#19307=CARTESIAN_POINT('Ctrl Pts',(97.4316120951221,0.906092089037131,2.00919444487641));
#19308=CARTESIAN_POINT('Ctrl Pts',(97.4307511257505,0.920459582804573,2.00265308175134));
#19309=CARTESIAN_POINT('Ctrl Pts',(97.4292120460474,0.946173980405307,1.99061040077821));
#19310=CARTESIAN_POINT('Ctrl Pts',(97.4285320450407,0.957546196822834,1.98516504579467));
#19311=CARTESIAN_POINT('Ctrl Pts',(97.4270849736607,0.981766270993176,1.9733112024035));
#19312=CARTESIAN_POINT('Ctrl Pts',(97.4263189379402,0.9945995425514,1.96687413823958));
#19313=CARTESIAN_POINT('Ctrl Pts',(97.424236575634,1.02950810950492,1.94893525144942));
#19314=CARTESIAN_POINT('Ctrl Pts',(97.4229290503544,1.05145324510039,1.93718396170564));
#19315=CARTESIAN_POINT('Ctrl Pts',(97.4136162113215,1.20777735362995,1.8500355021328));
#19316=CARTESIAN_POINT('Ctrl Pts',(97.4061362544506,1.3341230688445,1.76110170541595));
#19317=CARTESIAN_POINT('Ctrl Pts',(97.3921506410449,1.55202939370889,1.57070603299438));
#19318=CARTESIAN_POINT('Ctrl Pts',(97.3856525328407,1.64546921381575,1.47252692960714));
#19319=CARTESIAN_POINT('Ctrl Pts',(97.3776536859106,1.74053188733054,1.35221755567726));
#19320=CARTESIAN_POINT('Ctrl Pts',(97.3766996672777,1.75157697973595,1.33787952076132));
#19321=CARTESIAN_POINT('Ctrl Pts',(97.3752531158359,1.76785893318571,1.31619607968734));
#19322=CARTESIAN_POINT('Ctrl Pts',(97.3747691965829,1.7732295661026,1.30895157590678));
#19323=CARTESIAN_POINT('Ctrl Pts',(97.3738906425274,1.78283878667285,1.29582192422749));
#19324=CARTESIAN_POINT('Ctrl Pts',(97.3734970762231,1.78709313028584,1.28994834814982));
#19325=CARTESIAN_POINT('Ctrl Pts',(97.3726832838348,1.79578458564452,1.27782334024569));
#19326=CARTESIAN_POINT('Ctrl Pts',(97.372262845165,1.80021817800254,1.27156961068004));
#19327=CARTESIAN_POINT('Ctrl Pts',(97.3711593349858,1.81171037773796,1.25517890735915));
#19328=CARTESIAN_POINT('Ctrl Pts',(97.3704728686715,1.81871645182566,1.24500563680229));
#19329=CARTESIAN_POINT('Ctrl Pts',(97.3673409686397,1.85005898052567,1.19866513108422));
#19330=CARTESIAN_POINT('Ctrl Pts',(97.3648388381958,1.87340326183103,1.16184166105117));
#19331=CARTESIAN_POINT('Ctrl Pts',(97.3572567817081,1.9397248383195,1.05002467342151));
#19332=CARTESIAN_POINT('Ctrl Pts',(97.3520687270945,1.97939913373605,0.97317110919485));
#19333=CARTESIAN_POINT('Ctrl Pts',(97.3370987627309,2.08049131205197,0.745427948223738));
#19334=CARTESIAN_POINT('Ctrl Pts',(97.3273946107137,2.12985372372918,0.589784547703335));
#19335=CARTESIAN_POINT('Ctrl Pts',(97.31671785903,2.16698234211206,0.403183626600176));
#19336=CARTESIAN_POINT('Ctrl Pts',(97.3151929465046,2.17183590057099,0.376162763433086));
#19337=CARTESIAN_POINT('Ctrl Pts',(97.3127844093818,2.17877516558641,0.332900208248145));
#19338=CARTESIAN_POINT('Ctrl Pts',(97.3118906083612,2.18118678657203,0.316714371787064));
#19339=CARTESIAN_POINT('Ctrl Pts',(97.3103129998369,2.18515019370017,0.28791672815055));
#19340=CARTESIAN_POINT('Ctrl Pts',(97.3096269596416,2.18677358248112,0.275315672966913));
#19341=CARTESIAN_POINT('Ctrl Pts',(97.3081989327879,2.18994160626818,0.24892618186986));
#19342=CARTESIAN_POINT('Ctrl Pts',(97.3074576378885,2.19146518876689,0.235135750947186));
#19343=CARTESIAN_POINT('Ctrl Pts',(97.3055173658842,2.19513191861933,0.198807370926436));
#19344=CARTESIAN_POINT('Ctrl Pts',(97.3043252161215,2.19705823481799,0.176248897831331));
#19345=CARTESIAN_POINT('Ctrl Pts',(97.2984351380006,2.20492470471471,0.0636949522456942));
#19346=CARTESIAN_POINT('Ctrl Pts',(97.2939004399123,2.20568488556786,-0.026580008133357));
#19347=CARTESIAN_POINT('Ctrl Pts',(97.284847899904,2.19594817388748,-0.210280821575465));
#19348=CARTESIAN_POINT('Ctrl Pts',(97.2803469483846,2.18501646612491,-0.30349604135809));
#19349=CARTESIAN_POINT('Ctrl Pts',(97.2744798042756,2.16326590799182,-0.422665610385005));
#19350=CARTESIAN_POINT('Ctrl Pts',(97.2731504641328,2.15784857329439,-0.449505407251845));
#19351=CARTESIAN_POINT('Ctrl Pts',(97.2674275094161,2.13253171080127,-0.563902613953819));
#19352=CARTESIAN_POINT('Ctrl Pts',(97.2629636402508,2.10779366050144,-0.650292505246297));
#19353=CARTESIAN_POINT('Ctrl Pts',(97.2574446139191,2.07283845353986,-0.749121852516237));
#19354=CARTESIAN_POINT('Ctrl Pts',(97.2566444572458,2.0676714322159,-0.763267730248926));
#19355=CARTESIAN_POINT('Ctrl Pts',(97.2553881280853,2.05941634871663,-0.785168744517474));
#19356=CARTESIAN_POINT('Ctrl Pts',(97.2549376362427,2.05642841745628,-0.792961420220219));
#19357=CARTESIAN_POINT('Ctrl Pts',(97.2540986803974,2.05081487137384,-0.807356705823696));
#19358=CARTESIAN_POINT('Ctrl Pts',(97.2537109344989,2.0482015056176,-0.813963804443493));
#19359=CARTESIAN_POINT('Ctrl Pts',(97.2528101252096,2.04208622480996,-0.82920849017591));
#19360=CARTESIAN_POINT('Ctrl Pts',(97.2522957276487,2.03856143169631,-0.83783659056455));
#19361=CARTESIAN_POINT('Ctrl Pts',(97.2506426944887,2.02712632023857,-0.865328432133981));
#19362=CARTESIAN_POINT('Ctrl Pts',(97.2494925938245,2.01900829091629,-0.884103994845832));
#19363=CARTESIAN_POINT('Ctrl Pts',(97.2431087330273,1.97299224880633,-0.986590737798431));
#19364=CARTESIAN_POINT('Ctrl Pts',(97.2376507820627,1.93015138320509,-1.06797591797514));
#19365=CARTESIAN_POINT('Ctrl Pts',(97.2222497152123,1.79648599541898,-1.28744310928803));
#19366=CARTESIAN_POINT('Ctrl Pts',(97.2122882202069,1.69502612089247,-1.41836947935311));
#19367=CARTESIAN_POINT('Ctrl Pts',(97.2003226737584,1.54864880413619,-1.56885624138146));
#19368=CARTESIAN_POINT('Ctrl Pts',(97.197808430062,1.51643873872145,-1.60001155831753));
#19369=CARTESIAN_POINT('Ctrl Pts',(97.1943177112892,1.46964547271655,-1.64258910782558));
#19370=CARTESIAN_POINT('Ctrl Pts',(97.1933063696388,1.45583547398155,-1.65484135028619));
#19371=CARTESIAN_POINT('Ctrl Pts',(97.1916018293131,1.43213282904504,-1.67534396762353));
#19372=CARTESIAN_POINT('Ctrl Pts',(97.1909049442883,1.42231899901421,-1.68368361778125));
#19373=CARTESIAN_POINT('Ctrl Pts',(97.1894992233151,1.40227517390827,-1.70041624521519));
#19374=CARTESIAN_POINT('Ctrl Pts',(97.1887906123723,1.39204156156876,-1.70880407646227));
#19375=CARTESIAN_POINT('Ctrl Pts',(97.1870416364104,1.36646519368071,-1.72938512669559));
#19376=CARTESIAN_POINT('Ctrl Pts',(97.1860057473891,1.35103401675011,-1.74146695650532));
#19377=CARTESIAN_POINT('Ctrl Pts',(97.1820021835804,1.29032096800083,-1.78770942244571));
#19378=CARTESIAN_POINT('Ctrl Pts',(97.1790943708904,1.24388663194669,-1.82032412337711));
#19379=CARTESIAN_POINT('Ctrl Pts',(97.171457942478,1.11647080736586,-1.90266393335233));
#19380=CARTESIAN_POINT('Ctrl Pts',(97.1668356300204,1.0334466483486,-1.94900657013373));
#19381=CARTESIAN_POINT('Ctrl Pts',(97.1549936267287,0.812442913708665,-2.05426212987753));
#19382=CARTESIAN_POINT('Ctrl Pts',(97.1478555279512,0.670998777512727,-2.10471048877184));
#19383=CARTESIAN_POINT('Ctrl Pts',(97.1390379246194,0.507175503059395,-2.14493522842281));
#19384=CARTESIAN_POINT('Ctrl Pts',(97.1380377905056,0.4887404530414,-2.14921074983252));
#19385=CARTESIAN_POINT('Ctrl Pts',(97.1365412858173,0.461425898567661,-2.15517604359062));
#19386=CARTESIAN_POINT('Ctrl Pts',(97.136054764761,0.45258692827555,-2.15704953704731));
#19387=CARTESIAN_POINT('Ctrl Pts',(97.1351812347445,0.436797071893396,-2.16029500603582));
#19388=CARTESIAN_POINT('Ctrl Pts',(97.1347954099061,0.429850762167566,-2.16168788570218));
#19389=CARTESIAN_POINT('Ctrl Pts',(97.1339390981143,0.414496263369222,-2.16468984612883));
#19390=CARTESIAN_POINT('Ctrl Pts',(97.1334677839886,0.406085465510928,-2.16628342372901));
#19391=CARTESIAN_POINT('Ctrl Pts',(97.132079139233,0.381414181903443,-2.17080911702656));
#19392=CARTESIAN_POINT('Ctrl Pts',(97.1311547720636,0.365130098671784,-2.17360736529565));
#19393=CARTESIAN_POINT('Ctrl Pts',(97.1237607453317,0.235814081372858,-2.19433483245255));
#19394=CARTESIAN_POINT('Ctrl Pts',(97.1169153173528,0.12158207932078,-2.20361675603818));
#19395=CARTESIAN_POINT('Ctrl Pts',(97.0996910426312,-0.165204304117157,
-2.204548165254));
#19396=CARTESIAN_POINT('Ctrl Pts',(97.0893811162678,-0.337067250979015,
-2.18488659251315));
#19397=CARTESIAN_POINT('Ctrl Pts',(97.0782215230451,-0.530844126399516,
-2.13928280460057));
#19398=CARTESIAN_POINT('Ctrl Pts',(97.0767420311437,-0.556676601624274,
-2.13270664967745));
#19399=CARTESIAN_POINT('Ctrl Pts',(97.0743812852405,-0.598116721889119,
-2.1213529824741));
#19400=CARTESIAN_POINT('Ctrl Pts',(97.0734907216844,-0.613801128296913,
-2.11686803659208));
#19401=CARTESIAN_POINT('Ctrl Pts',(97.0719189369909,-0.641569560307601,
-2.10859309335856));
#19402=CARTESIAN_POINT('Ctrl Pts',(97.0712354956868,-0.653673300649765,
-2.10487233803667));
#19403=CARTESIAN_POINT('Ctrl Pts',(97.0698014477056,-0.679128519827647,
-2.09680651736959));
#19404=CARTESIAN_POINT('Ctrl Pts',(97.0690516546659,-0.692471932264333,
-2.09243775373208));
#19405=CARTESIAN_POINT('Ctrl Pts',(97.0670626270685,-0.727951297086907,
-2.08044490251017));
#19406=CARTESIAN_POINT('Ctrl Pts',(97.0658308738873,-0.750009361629385,
-2.07259501500504));
#19407=CARTESIAN_POINT('Ctrl Pts',(97.0592162345691,-0.86882727410245,-2.02816545960972));
#19408=CARTESIAN_POINT('Ctrl Pts',(97.0540527908047,-0.963049890183291,
-1.98515844605545));
#19409=CARTESIAN_POINT('Ctrl Pts',(97.0421462615306,-1.17691867928918,-1.86871469878127));
#19410=CARTESIAN_POINT('Ctrl Pts',(97.0355255214351,-1.29325484426941,-1.79017330698028));
#19411=CARTESIAN_POINT('Ctrl Pts',(97.025640897626,-1.4464206216406,-1.6639993180996));
#19412=CARTESIAN_POINT('Ctrl Pts',(97.0226711478744,-1.48999761786776,-1.62509458126694));
#19413=CARTESIAN_POINT('Ctrl Pts',(97.0188499845982,-1.54203549182178,-1.57478200638507));
#19414=CARTESIAN_POINT('Ctrl Pts',(97.0181048472828,-1.55200282918893,-1.56495975146903));
#19415=CARTESIAN_POINT('Ctrl Pts',(97.0169211398444,-1.56753818592971,-1.54935613902266));
#19416=CARTESIAN_POINT('Ctrl Pts',(97.0164873571561,-1.57316947394977,-1.54363797956024));
#19417=CARTESIAN_POINT('Ctrl Pts',(97.0156611581329,-1.58377475884756,-1.53275078596568));
#19418=CARTESIAN_POINT('Ctrl Pts',(97.0152692240696,-1.58875490101081,-1.52758807200213));
#19419=CARTESIAN_POINT('Ctrl Pts',(97.0143331121053,-1.60053126483617,-1.51526010963161));
#19420=CARTESIAN_POINT('Ctrl Pts',(97.013787237835,-1.60730464945964,-1.50807336882887));
#19421=CARTESIAN_POINT('Ctrl Pts',(97.011921630882,-1.63014696792455,-1.48350836770117));
#19422=CARTESIAN_POINT('Ctrl Pts',(97.0105860971985,-1.64598365414263,-1.46591743693378));
#19423=CARTESIAN_POINT('Ctrl Pts',(97.0072542851199,-1.68432873688188,-1.42191998914543));
#19424=CARTESIAN_POINT('Ctrl Pts',(97.0052405753113,-1.7065023690532,-1.39523087466689));
#19425=CARTESIAN_POINT('Ctrl Pts',(96.9962662902311,-1.8014176255517,-1.27533814017816));
#19426=CARTESIAN_POINT('Ctrl Pts',(96.9890946346091,-1.86722085702178,-1.17689352755256));
#19427=CARTESIAN_POINT('Ctrl Pts',(96.9741668754745,-1.98885785406354,-0.958825723636734));
#19428=CARTESIAN_POINT('Ctrl Pts',(96.9664720159661,-2.04251020879749,-0.838488811851101));
#19429=CARTESIAN_POINT('Ctrl Pts',(96.9577872296081,-2.09301853508694,-0.691002142353862));
#19430=CARTESIAN_POINT('Ctrl Pts',(96.9564413074771,-2.1005353192608,-0.66780385514399));
#19431=CARTESIAN_POINT('Ctrl Pts',(96.9543213976161,-2.11187238155074,-0.63072814141938));
#19432=CARTESIAN_POINT('Ctrl Pts',(96.9535392432522,-2.115944230563,-0.616930280738423));
#19433=CARTESIAN_POINT('Ctrl Pts',(96.9520865245355,-2.12329703367339,-0.59108508282144));
#19434=CARTESIAN_POINT('Ctrl Pts',(96.9514149004651,-2.12661125467023,-0.579047881231763));
#19435=CARTESIAN_POINT('Ctrl Pts',(96.949907010506,-2.13385775329934,-0.551827029625656));
#19436=CARTESIAN_POINT('Ctrl Pts',(96.9490726946477,-2.13773061909298,-0.536628176097042));
#19437=CARTESIAN_POINT('Ctrl Pts',(96.9465838312718,-2.14886712830983,-0.490888474847003));
#19438=CARTESIAN_POINT('Ctrl Pts',(96.9449449579582,-2.1556410191943,-0.46023185000507));
#19439=CARTESIAN_POINT('Ctrl Pts',(96.9412043435341,-2.16976503490574,-0.389132957326647));
#19440=CARTESIAN_POINT('Ctrl Pts',(96.9391169142962,-2.17664352550493,-0.348608626618659));
#19441=CARTESIAN_POINT('Ctrl Pts',(96.9316231066508,-2.19752021254047,-0.200642120853897));
#19442=CARTESIAN_POINT('Ctrl Pts',(96.9263927060389,-2.2047260212634,-0.0923963498250632));
#19443=CARTESIAN_POINT('Ctrl Pts',(96.9149491386593,-2.20301337828792,0.144365336625957));
#19444=CARTESIAN_POINT('Ctrl Pts',(96.9087549236805,-2.19086155438656,0.272447760188528));
#19445=CARTESIAN_POINT('Ctrl Pts',(96.9009999229888,-2.16395445665159,0.418724895336054));
#19446=CARTESIAN_POINT('Ctrl Pts',(96.8999273359669,-2.15999958350712,0.438669772878307));
#19447=CARTESIAN_POINT('Ctrl Pts',(96.8983481789791,-2.15385548233814,0.46755447876192));
#19448=CARTESIAN_POINT('Ctrl Pts',(96.8978532630552,-2.15188519948143,0.476540356693368));
#19449=CARTESIAN_POINT('Ctrl Pts',(96.8969702426759,-2.14829278082196,0.492447624207584));
#19450=CARTESIAN_POINT('Ctrl Pts',(96.896583421801,-2.14669333460649,0.4993738684383));
#19451=CARTESIAN_POINT('Ctrl Pts',(96.8957395105099,-2.14314878268371,0.514391429695719));
#19452=CARTESIAN_POINT('Ctrl Pts',(96.8952817597846,-2.14119138197548,0.522479385957936));
#19453=CARTESIAN_POINT('Ctrl Pts',(96.8939712565482,-2.13548737806627,0.545477787444204));
#19454=CARTESIAN_POINT('Ctrl Pts',(96.8931125783017,-2.13163057194366,0.560360095056632));
#19455=CARTESIAN_POINT('Ctrl Pts',(96.8857937074348,-2.09772639900901,0.685768814422898));
#19456=CARTESIAN_POINT('Ctrl Pts',(96.8789488925895,-2.05926333488053,0.793829090874947));
#19457=CARTESIAN_POINT('Ctrl Pts',(96.8615781791956,-1.94135202668963,1.05797236852256));
#19458=CARTESIAN_POINT('Ctrl Pts',(96.8511180712936,-1.85138214638012,1.20853500191345));
#19459=CARTESIAN_POINT('Ctrl Pts',(96.8398459112401,-1.72845073171139,1.3677604339701));
#19460=CARTESIAN_POINT('Ctrl Pts',(96.8383834749853,-1.71197201899801,1.38833080630519));
#19461=CARTESIAN_POINT('Ctrl Pts',(96.836044389006,-1.68475791676177,1.42108058475099));
#19462=CARTESIAN_POINT('Ctrl Pts',(96.8351587018626,-1.67425034717578,1.43344517205792));
#19463=CARTESIAN_POINT('Ctrl Pts',(96.8335923690952,-1.65530791671741,1.45524285891229));
#19464=CARTESIAN_POINT('Ctrl Pts',(96.8329095577253,-1.64692664539698,1.46472137676814));
#19465=CARTESIAN_POINT('Ctrl Pts',(96.8315109868719,-1.62950665573687,1.48408335917156));
#19466=CARTESIAN_POINT('Ctrl Pts',(96.8307956659667,-1.62045852628863,1.49395767459595));
#19467=CARTESIAN_POINT('Ctrl Pts',(96.8289102063897,-1.59624614406658,1.51990210682352));
#19468=CARTESIAN_POINT('Ctrl Pts',(96.8277466493144,-1.58092908860251,1.53582792992859));
#19469=CARTESIAN_POINT('Ctrl Pts',(96.8251969752012,-1.54655618885523,1.57050774755632));
#19470=CARTESIAN_POINT('Ctrl Pts',(96.8238156283288,-1.52739326353589,1.58915088181764));
#19471=CARTESIAN_POINT('Ctrl Pts',(96.819655796705,-1.46811351932416,1.64475953931745));
#19472=CARTESIAN_POINT('Ctrl Pts',(96.8169208210087,-1.42695850217705,1.68058953576053));
#19473=CARTESIAN_POINT('Ctrl Pts',(96.807027457737,-1.27125284246115,1.80630074056778));
#19474=CARTESIAN_POINT('Ctrl Pts',(96.80015139719,-1.14921571393859,1.8862946513986));
#19475=CARTESIAN_POINT('Ctrl Pts',(96.789285822506,-0.953514715746994,1.98848759794431));
#19476=CARTESIAN_POINT('Ctrl Pts',(96.7855087122296,-0.885110091611861,
2.01986418848735));
#19477=CARTESIAN_POINT('Ctrl Pts',(96.7807700852478,-0.801544905065273,
2.05313397816844));
#19478=CARTESIAN_POINT('Ctrl Pts',(96.7799863413842,-0.787793198429323,
2.05844971285503));
#19479=CARTESIAN_POINT('Ctrl Pts',(96.7787504074862,-0.766241425292141,
2.06653297989104));
#19480=CARTESIAN_POINT('Ctrl Pts',(96.7783036083793,-0.75847710412266,2.06939531187093));
#19481=CARTESIAN_POINT('Ctrl Pts',(96.7775065015081,-0.744677819527043,
2.07439435261396));
#19482=CARTESIAN_POINT('Ctrl Pts',(96.7771572354373,-0.73864942056618,2.07654858246399));
#19483=CARTESIAN_POINT('Ctrl Pts',(96.776312246932,-0.724107193986955,2.08167386562238));
#19484=CARTESIAN_POINT('Ctrl Pts',(96.7758150313979,-0.715584498214399,
2.08461894149664));
#19485=CARTESIAN_POINT('Ctrl Pts',(96.7742707294686,-0.689210140576254,
2.09355198637103));
#19486=CARTESIAN_POINT('Ctrl Pts',(96.7732141265929,-0.671300079510141,
2.09936340170609));
#19487=CARTESIAN_POINT('Ctrl Pts',(96.7677908761509,-0.579917841186144,
2.12772600150341));
#19488=CARTESIAN_POINT('Ctrl Pts',(96.7632639579809,-0.50538159200088,2.14665091485491));
#19489=CARTESIAN_POINT('Ctrl Pts',(96.7500988493336,-0.288979019454966,
2.18969993523615));
#19490=CARTESIAN_POINT('Ctrl Pts',(96.7413697229979,-0.145521252649599,
2.20388829904848));
#19491=CARTESIAN_POINT('Ctrl Pts',(96.7329771885798,-0.00170172224861046,
2.20399934304468));
#19492=CARTESIAN_POINT('Ctrl Pts',(96.7329771495123,-0.00170105276327685,
2.20399934356149));
#19493=CARTESIAN_POINT('Ctrl Pts',(96.7329440613314,-0.00113403367530617,
2.20399978118839));
#19494=CARTESIAN_POINT('Ctrl Pts',(96.7329109782893,-0.000567016049827459,
2.204));
#19495=CARTESIAN_POINT('Ctrl Pts',(96.7328779004031,-1.24027783152639E-11,
2.204));
#19496=CARTESIAN_POINT('',(96.6271339259349,-0.00170191538198742,2.20399918312151));
#19497=CARTESIAN_POINT('Ctrl Pts',(96.6270503826334,2.66056133811156E-11,
2.204));
#19498=CARTESIAN_POINT('Ctrl Pts',(96.6270783363781,-0.000567503799259821,
2.20400000000001));
#19499=CARTESIAN_POINT('Ctrl Pts',(96.6271062864288,-0.00113501110448395,
2.20399978081177));
#19500=CARTESIAN_POINT('Ctrl Pts',(96.627134232812,-0.00170252176299227,
2.20399934242723));
#19501=CARTESIAN_POINT('Ctrl Pts',(96.6271342022874,-0.00170190189588519,
2.20399934290597));
#19502=CARTESIAN_POINT('Ctrl Pts',(96.632608601421,-0.112871190563222,2.2039134993127));
#19503=CARTESIAN_POINT('Ctrl Pts',(96.6379179252564,-0.223874109134158,
2.19541691506186));
#19504=CARTESIAN_POINT('Ctrl Pts',(96.6478313048556,-0.425361057701924,
2.16454869528108));
#19505=CARTESIAN_POINT('Ctrl Pts',(96.6523990936831,-0.515974735017222,
2.14475406912885));
#19506=CARTESIAN_POINT('Ctrl Pts',(96.6583017855094,-0.624887365886604,
2.11365956383491));
#19507=CARTESIAN_POINT('Ctrl Pts',(96.6593888179286,-0.644629080381249,
2.10772252923118));
#19508=CARTESIAN_POINT('Ctrl Pts',(96.6609936748519,-0.673251137647653,
2.09867514198364));
#19509=CARTESIAN_POINT('Ctrl Pts',(96.6614995840245,-0.682199976442728,
2.0957832978501));
#19510=CARTESIAN_POINT('Ctrl Pts',(96.6623974544973,-0.697944776315688,
2.09058379336497));
#19511=CARTESIAN_POINT('Ctrl Pts',(96.6627880254367,-0.70474836211065,2.08830008677232));
#19512=CARTESIAN_POINT('Ctrl Pts',(96.6636426490523,-0.719535401113837,
2.0832561426042));
#19513=CARTESIAN_POINT('Ctrl Pts',(96.6641074033534,-0.727514065034906,
2.08048326824711));
#19514=CARTESIAN_POINT('Ctrl Pts',(96.6654206156671,-0.74989035794726,2.07256224181435));
#19515=CARTESIAN_POINT('Ctrl Pts',(96.6662748224616,-0.764250368225651,
2.06731012264312));
#19516=CARTESIAN_POINT('Ctrl Pts',(96.6730866049203,-0.877346079311855,
2.02460643001447));
#19517=CARTESIAN_POINT('Ctrl Pts',(96.6793714753231,-0.97332057428682,1.980255095452));
#19518=CARTESIAN_POINT('Ctrl Pts',(96.6926802781187,-1.16750519081809,1.87298291856154));
#19519=CARTESIAN_POINT('Ctrl Pts',(96.6996897043096,-1.26467249081611,1.80879521967758));
#19520=CARTESIAN_POINT('Ctrl Pts',(96.7096058907678,-1.39831625982184,1.70445464433301));
#19521=CARTESIAN_POINT('Ctrl Pts',(96.7126768165444,-1.43910667999149,1.67015765274309));
#19522=CARTESIAN_POINT('Ctrl Pts',(96.7178409275878,-1.50677264015792,1.60894183232749));
#19523=CARTESIAN_POINT('Ctrl Pts',(96.7199607877324,-1.53426705887712,1.58274522680123));
#19524=CARTESIAN_POINT('Ctrl Pts',(96.7228958098586,-1.57191868049542,1.54496723133478));
#19525=CARTESIAN_POINT('Ctrl Pts',(96.7237362899108,-1.58265126217805,1.53397101771918));
#19526=CARTESIAN_POINT('Ctrl Pts',(96.7245977770186,-1.59359891095592,1.52251723803876));
#19527=CARTESIAN_POINT('Ctrl Pts',(96.7246237984946,-1.59392953755357,1.52217110025116));
#19528=CARTESIAN_POINT('Ctrl Pts',(96.7246765545904,-1.59459974951247,1.52146898781758));
#19529=CARTESIAN_POINT('Ctrl Pts',(96.724703288933,-1.59493932850801,1.52111300711513));
#19530=CARTESIAN_POINT('Ctrl Pts',(96.7247576031014,-1.59562911724371,1.52038941655998));
#19531=CARTESIAN_POINT('Ctrl Pts',(96.7247851825895,-1.59597931921882,1.52002179932065));
#19532=CARTESIAN_POINT('Ctrl Pts',(96.7248413363122,-1.59669223828425,1.51927290936653));
#19533=CARTESIAN_POINT('Ctrl Pts',(96.7248699101362,-1.59705494592726,1.51889162767531));
#19534=CARTESIAN_POINT('Ctrl Pts',(96.7249282225963,-1.59779502175202,1.51811309482505));
#19535=CARTESIAN_POINT('Ctrl Pts',(96.7249579607335,-1.59817237844339,1.51771583275533));
#19536=CARTESIAN_POINT('Ctrl Pts',(96.7250187975307,-1.59894421956128,1.51690267035238));
#19537=CARTESIAN_POINT('Ctrl Pts',(96.7250498955828,-1.59933868997506,1.51648675673094));
#19538=CARTESIAN_POINT('Ctrl Pts',(96.7250928023211,-1.59988284951363,1.51591256848462));
#19539=CARTESIAN_POINT('Ctrl Pts',(96.7251046170066,-1.60003267727788,1.51575442572354));
#19540=CARTESIAN_POINT('Ctrl Pts',(96.7251320127,-1.60038007086697,1.51538764391634));
#19541=CARTESIAN_POINT('Ctrl Pts',(96.7251475929585,-1.60057761937088,1.51517898841412));
#19542=CARTESIAN_POINT('Ctrl Pts',(96.7251839639256,-1.60103873885075,1.51469175206577));
#19543=CARTESIAN_POINT('Ctrl Pts',(96.7252047532565,-1.60130227797765,1.51441314099579));
#19544=CARTESIAN_POINT('Ctrl Pts',(96.7259092265188,-1.61023152824141,1.50496828539381));
#19545=CARTESIAN_POINT('Ctrl Pts',(96.7265895026541,-1.61881858344139,1.49572775521251));
#19546=CARTESIAN_POINT('Ctrl Pts',(96.7280451287541,-1.63711293485152,1.47569909868651));
#19547=CARTESIAN_POINT('Ctrl Pts',(96.7288193512651,-1.64679399974583,1.46488775252045));
#19548=CARTESIAN_POINT('Ctrl Pts',(96.7308915050293,-1.67256366980744,1.43553108383457));
#19549=CARTESIAN_POINT('Ctrl Pts',(96.7321810891175,-1.6884505913895,1.41681099170187));
#19550=CARTESIAN_POINT('Ctrl Pts',(96.7401767529182,-1.78589772233918,1.29801816504647));
#19551=CARTESIAN_POINT('Ctrl Pts',(96.7465282937912,-1.85884928113737,1.19120362383043));
#19552=CARTESIAN_POINT('Ctrl Pts',(96.7573557862813,-1.96815903338244,0.996417738584225));
#19553=CARTESIAN_POINT('Ctrl Pts',(96.761869776937,-2.00896108881992,0.911357619124146));
#19554=CARTESIAN_POINT('Ctrl Pts',(96.7690085482016,-2.06315811919891,0.776896571692167));
#19555=CARTESIAN_POINT('Ctrl Pts',(96.7715421473601,-2.08049259709879,0.729204857658749));
#19556=CARTESIAN_POINT('Ctrl Pts',(96.7752295517117,-2.10270124374175,0.660841115319203));
#19557=CARTESIAN_POINT('Ctrl Pts',(96.7763265038397,-2.10894696041381,0.640629503795274));
#19558=CARTESIAN_POINT('Ctrl Pts',(96.7782946067704,-2.11949164736252,0.604679444358499));
#19559=CARTESIAN_POINT('Ctrl Pts',(96.779159915934,-2.12390867252279,0.588977073682936));
#19560=CARTESIAN_POINT('Ctrl Pts',(96.7804943751342,-2.13037936283693,0.564954145421908));
#19561=CARTESIAN_POINT('Ctrl Pts',(96.7809565875128,-2.13255955115943,0.556667918760472));
#19562=CARTESIAN_POINT('Ctrl Pts',(96.7818103938466,-2.13647374436715,0.541430753199892));
#19563=CARTESIAN_POINT('Ctrl Pts',(96.7822011589115,-2.13822224176788,0.534483827163808));
#19564=CARTESIAN_POINT('Ctrl Pts',(96.7831003291304,-2.14214800019384,0.518558857447746));
#19565=CARTESIAN_POINT('Ctrl Pts',(96.7836099773771,-2.1443026982404,0.50957558359606));
#19566=CARTESIAN_POINT('Ctrl Pts',(96.7852164928162,-2.1508779529591,0.481381978685206));
#19567=CARTESIAN_POINT('Ctrl Pts',(96.7863238778525,-2.15509718384751,0.462126228467932));
#19568=CARTESIAN_POINT('Ctrl Pts',(96.7954033472618,-2.1872357871918,0.305427045769771));
#19569=CARTESIAN_POINT('Ctrl Pts',(96.8039015004029,-2.20223396910464,0.165670333820707));
#19570=CARTESIAN_POINT('Ctrl Pts',(96.8212496308491,-2.20557267074338,-0.123476300175564));
#19571=CARTESIAN_POINT('Ctrl Pts',(96.8300336253042,-2.19219320486518,-0.272211415067468));
#19572=CARTESIAN_POINT('Ctrl Pts',(96.8397474961803,-2.15911116626638,-0.443275148117128));
#19573=CARTESIAN_POINT('Ctrl Pts',(96.8411422515811,-2.15388966926638,-0.467988517811588));
#19574=CARTESIAN_POINT('Ctrl Pts',(96.8433177788552,-2.14499806131925,-0.506764519960096));
#19575=CARTESIAN_POINT('Ctrl Pts',(96.8441075472288,-2.14161182432808,-0.520889402720316));
#19576=CARTESIAN_POINT('Ctrl Pts',(96.8455812737711,-2.13499525557279,-0.547332995751281));
#19577=CARTESIAN_POINT('Ctrl Pts',(96.8462662420241,-2.13179732235706,-0.559659124288174));
#19578=CARTESIAN_POINT('Ctrl Pts',(96.8477996890475,-2.12436202988242,-0.587328975223473));
#19579=CARTESIAN_POINT('Ctrl Pts',(96.8486461929131,-2.12006489052959,-0.602655985702586));
#19580=CARTESIAN_POINT('Ctrl Pts',(96.851129068441,-2.10689321662102,-0.647751348012335));
#19581=CARTESIAN_POINT('Ctrl Pts',(96.8527503672805,-2.09755482642524,-0.677380772237077));
#19582=CARTESIAN_POINT('Ctrl Pts',(96.8616122968508,-2.04247638475602,-0.84005865737921));
#19583=CARTESIAN_POINT('Ctrl Pts',(96.8684440770106,-1.98470461317013,-0.968690146620194));
#19584=CARTESIAN_POINT('Ctrl Pts',(96.8801631542396,-1.86469323380246,-1.17935948782349));
#19585=CARTESIAN_POINT('Ctrl Pts',(96.885059729989,-1.80826769929528,-1.26417373357032));
#19586=CARTESIAN_POINT('Ctrl Pts',(96.89179893821,-1.72655025242824,-1.37028328134208));
#19587=CARTESIAN_POINT('Ctrl Pts',(96.8934405196446,-1.70635530487693,-1.39535065326524));
#19588=CARTESIAN_POINT('Ctrl Pts',(96.8962783448656,-1.67116520247631,-1.4371242852469));
#19589=CARTESIAN_POINT('Ctrl Pts',(96.8974586892698,-1.65645022292543,-1.45406049655015));
#19590=CARTESIAN_POINT('Ctrl Pts',(96.8991761491611,-1.63498930339738,-1.47801237445083));
#19591=CARTESIAN_POINT('Ctrl Pts',(96.8996988765888,-1.62845100103476,-1.48521309289721));
#19592=CARTESIAN_POINT('Ctrl Pts',(96.9006153981239,-1.61698203136213,-1.49767724240482));
#19593=CARTESIAN_POINT('Ctrl Pts',(96.9010075909095,-1.61207286349252,-1.5029601105726));
#19594=CARTESIAN_POINT('Ctrl Pts',(96.9018525612768,-1.60149500303637,-1.51423173554284));
#19595=CARTESIAN_POINT('Ctrl Pts',(96.9023058945727,-1.59581869659414,-1.52021270772353));
#19596=CARTESIAN_POINT('Ctrl Pts',(96.9035572835009,-1.5801418718059,-1.53654640484188));
#19597=CARTESIAN_POINT('Ctrl Pts',(96.9043602930301,-1.57007345824655,-1.54683305582083));
#19598=CARTESIAN_POINT('Ctrl Pts',(96.908933751301,-1.51263189462613,-1.60438106099893));
#19599=CARTESIAN_POINT('Ctrl Pts',(96.9128366591611,-1.46322985090542,-1.64956076996027));
#19600=CARTESIAN_POINT('Ctrl Pts',(96.9244021095839,-1.31338961811199,-1.77456084169117));
#19601=CARTESIAN_POINT('Ctrl Pts',(96.9321959358845,-1.20794413543602,-1.84795320428208));
#19602=CARTESIAN_POINT('Ctrl Pts',(96.9460332677269,-1.00536352258569,-1.9641667567872));
#19603=CARTESIAN_POINT('Ctrl Pts',(96.9521263590037,-0.910367205245671,
-2.00996101675701));
#19604=CARTESIAN_POINT('Ctrl Pts',(96.9593017337332,-0.790463425678604,
-2.05750891647851));
#19605=CARTESIAN_POINT('Ctrl Pts',(96.960605655235,-0.768338510283478,-2.06587302705679));
#19606=CARTESIAN_POINT('Ctrl Pts',(96.9626724093394,-0.732738520079864,
-2.07868019947362));
#19607=CARTESIAN_POINT('Ctrl Pts',(96.9634427936861,-0.719348185310399,
-2.08335194146431));
#19608=CARTESIAN_POINT('Ctrl Pts',(96.9648999020293,-0.693795921853906,
-2.0919911181715));
#19609=CARTESIAN_POINT('Ctrl Pts',(96.9655873952018,-0.681642767865331,
-2.09598253004958));
#19610=CARTESIAN_POINT('Ctrl Pts',(96.9671529231258,-0.653750082155866,
-2.10487495022109));
#19611=CARTESIAN_POINT('Ctrl Pts',(96.9680286232363,-0.63798883693985,-2.10970566427644));
#19612=CARTESIAN_POINT('Ctrl Pts',(96.9707535716296,-0.58846174028786,-2.12427958380524));
#19613=CARTESIAN_POINT('Ctrl Pts',(96.9725824343572,-0.554515344022683,
-2.13339257573941));
#19614=CARTESIAN_POINT('Ctrl Pts',(96.9834267738383,-0.349418258915584,
-2.1832248004513));
#19615=CARTESIAN_POINT('Ctrl Pts',(96.9917799621534,-0.174120346396682,
-2.20414351491874));
#19616=CARTESIAN_POINT('Ctrl Pts',(97.0049604920597,0.0971591693623677,
-2.20392107304026));
#19617=CARTESIAN_POINT('Ctrl Pts',(97.0096515444659,0.192397192657645,-2.19765510492763));
#19618=CARTESIAN_POINT('Ctrl Pts',(97.0157052999137,0.307624569032217,-2.18252587211148));
#19619=CARTESIAN_POINT('Ctrl Pts',(97.0168060435193,0.32828844823504,-2.17951340672665));
#19620=CARTESIAN_POINT('Ctrl Pts',(97.0184274893463,0.358239390798993,-2.17471145142811));
#19621=CARTESIAN_POINT('Ctrl Pts',(97.0189359270168,0.367563235036731,-2.17315499210909));
#19622=CARTESIAN_POINT('Ctrl Pts',(97.019833077463,0.383888895198691,-2.17032162811321));
#19623=CARTESIAN_POINT('Ctrl Pts',(97.0202203330934,0.390894957635741,-2.16907071900586));
#19624=CARTESIAN_POINT('Ctrl Pts',(97.0210682396807,0.406144101216154,-2.16627175318586));
#19625=CARTESIAN_POINT('Ctrl Pts',(97.021529587742,0.41438431775802,-2.16471059775278));
#19626=CARTESIAN_POINT('Ctrl Pts',(97.0228242546749,0.4373577393494,-2.16022217468882));
#19627=CARTESIAN_POINT('Ctrl Pts',(97.0236630784208,0.452069957475402,-2.15719131382255));
#19628=CARTESIAN_POINT('Ctrl Pts',(97.0292626515689,0.549243059122469,-2.13613500468892));
#19629=CARTESIAN_POINT('Ctrl Pts',(97.0342335472769,0.630634372245638,-2.11353693434011));
#19630=CARTESIAN_POINT('Ctrl Pts',(97.041116723865,0.739778607725766,-2.07636675175192));
#19631=CARTESIAN_POINT('Ctrl Pts',(97.0429704294909,0.768822906975942,-2.06578860844319));
#19632=CARTESIAN_POINT('Ctrl Pts',(97.0503214017933,0.882932866118027,-2.02148902226851));
#19633=CARTESIAN_POINT('Ctrl Pts',(97.0558255421417,0.96608978979318,-1.98309359730076));
#19634=CARTESIAN_POINT('Ctrl Pts',(97.0667400773437,1.12909288601398,-1.89513775357621));
#19635=CARTESIAN_POINT('Ctrl Pts',(97.0721334573602,1.20864898903318,-1.84541837313117));
#19636=CARTESIAN_POINT('Ctrl Pts',(97.0786212759344,1.30349829395804,-1.77736812486294));
#19637=CARTESIAN_POINT('Ctrl Pts',(97.0798887196036,1.32197992795045,-1.76366504201175));
#19638=CARTESIAN_POINT('Ctrl Pts',(97.0819117049338,1.35139214437696,-1.74113539688895));
#19639=CARTESIAN_POINT('Ctrl Pts',(97.0826742465388,1.36245845850767,-1.73248958434262));
#19640=CARTESIAN_POINT('Ctrl Pts',(97.0841252237058,1.38347280620687,-1.71574575721257));
#19641=CARTESIAN_POINT('Ctrl Pts',(97.0848143262208,1.39343422448967,-1.70766553533358));
#19642=CARTESIAN_POINT('Ctrl Pts',(97.0863807290431,1.41603009739407,-1.68900747670599));
#19643=CARTESIAN_POINT('Ctrl Pts',(97.0872557194261,1.4286176818724,-1.67837392497714));
#19644=CARTESIAN_POINT('Ctrl Pts',(97.0900294886792,1.46839463477093,-1.64399999082385));
#19645=CARTESIAN_POINT('Ctrl Pts',(97.091906452713,1.49512126406873,-1.6197318828176));
#19646=CARTESIAN_POINT('Ctrl Pts',(97.1027342386393,1.64777465345655,-1.4741211198295));
#19647=CARTESIAN_POINT('Ctrl Pts',(97.111036359595,1.7594917697619,-1.33880015054082));
#19648=CARTESIAN_POINT('Ctrl Pts',(97.1241510822338,1.90542219097849,-1.11176029859333));
#19649=CARTESIAN_POINT('Ctrl Pts',(97.1288268912561,1.95157136135416,-1.02859641079584));
#19650=CARTESIAN_POINT('Ctrl Pts',(97.1348619589028,2.00112471832434,-0.923877996788937));
#19651=CARTESIAN_POINT('Ctrl Pts',(97.1359610220495,2.00977445259573,-0.904907331524308));
#19652=CARTESIAN_POINT('Ctrl Pts',(97.1375804355341,2.02195033961223,-0.877167071072994));
#19653=CARTESIAN_POINT('Ctrl Pts',(97.1380885643828,2.02569150324292,-0.868492471769706));
#19654=CARTESIAN_POINT('Ctrl Pts',(97.1389853746996,2.03215290966729,-0.853241581537137));
#19655=CARTESIAN_POINT('Ctrl Pts',(97.1393726028778,2.03489723787633,-0.846675778941045));
#19656=CARTESIAN_POINT('Ctrl Pts',(97.1402207007066,2.04080809714263,-0.83233930320665));
#19657=CARTESIAN_POINT('Ctrl Pts',(97.1406822702671,2.04396202021073,-0.8245639212205));
#19658=CARTESIAN_POINT('Ctrl Pts',(97.141978140253,2.0526445202068,-0.802802986094939));
#19659=CARTESIAN_POINT('Ctrl Pts',(97.1428179612323,2.05807436467379,-0.788778831424574));
#19660=CARTESIAN_POINT('Ctrl Pts',(97.1484550104124,2.09325585346522,-0.695075432104919));
#19661=CARTESIAN_POINT('Ctrl Pts',(97.1534655674885,2.11851480296155,-0.6137933669029));
#19662=CARTESIAN_POINT('Ctrl Pts',(97.1603327832216,2.14623711295988,-0.502175831762616));
#19663=CARTESIAN_POINT('Ctrl Pts',(97.16213035524,2.1528675169356,-0.472943685966584));
#19664=CARTESIAN_POINT('Ctrl Pts',(97.1693631031807,2.17710796390953,-0.354967187465543));
#19665=CARTESIAN_POINT('Ctrl Pts',(97.174805668844,2.18984334957001,-0.265307757864347));
#19666=CARTESIAN_POINT('Ctrl Pts',(97.1838555687657,2.20203854153165,-0.112305641845383));
#19667=CARTESIAN_POINT('Ctrl Pts',(97.1875156020542,2.20434939746418,-0.0493053001917814));
#19668=CARTESIAN_POINT('Ctrl Pts',(97.1935536373236,2.20368886979997,0.0568660252298257));
#19669=CARTESIAN_POINT('Ctrl Pts',(97.1959711269057,2.20215297016257,0.10000521861277));
#19670=CARTESIAN_POINT('Ctrl Pts',(97.1993324559348,2.19819328859719,0.160874041877885));
#19671=CARTESIAN_POINT('Ctrl Pts',(97.200308661995,2.19681925300165,0.178659977188884));
#19672=CARTESIAN_POINT('Ctrl Pts',(97.2019842072095,2.19407144129111,0.209368877241939));
#19673=CARTESIAN_POINT('Ctrl Pts',(97.2026866898402,2.19279903907687,0.222299798888353));
#19674=CARTESIAN_POINT('Ctrl Pts',(97.2041181766385,2.18995881683217,0.248760673481563));
#19675=CARTESIAN_POINT('Ctrl Pts',(97.2048467953177,2.18837977733654,0.262288874490857));
#19676=CARTESIAN_POINT('Ctrl Pts',(97.2066901966621,2.18404461340287,0.296659922797866));
#19677=CARTESIAN_POINT('Ctrl Pts',(97.2077994953409,2.1811154477108,0.31747980634697));
#19678=CARTESIAN_POINT('Ctrl Pts',(97.212184735964,2.16825640628148,0.400274014343198));
#19679=CARTESIAN_POINT('Ctrl Pts',(97.2153869030998,2.15597888599049,0.461856116178701));
#19680=CARTESIAN_POINT('Ctrl Pts',(97.2259518493747,2.10590445597134,0.666918872713687));
#19681=CARTESIAN_POINT('Ctrl Pts',(97.2329834075584,2.05626755979001,0.807080093503427));
#19682=CARTESIAN_POINT('Ctrl Pts',(97.2447858205727,1.95292685016179,1.02589842417721));
#19683=CARTESIAN_POINT('Ctrl Pts',(97.2494320307433,1.90756869800671,1.10795710403447));
#19684=CARTESIAN_POINT('Ctrl Pts',(97.2551597798963,1.84900030694052,1.1996007809649));
#19685=CARTESIAN_POINT('Ctrl Pts',(97.2559626175308,1.84073558702578,1.21224446477707));
#19686=CARTESIAN_POINT('Ctrl Pts',(97.2572202021618,1.82772106692227,1.23171459301282));
#19687=CARTESIAN_POINT('Ctrl Pts',(97.2576691888672,1.82306133985835,1.23860101873783));
#19688=CARTESIAN_POINT('Ctrl Pts',(97.2585117882168,1.81429538068962,1.25139924924421));
#19689=CARTESIAN_POINT('Ctrl Pts',(97.2589047532771,1.81019902687534,1.2573174966686));
#19690=CARTESIAN_POINT('Ctrl Pts',(97.2598178553037,1.80066095528577,1.27095448952557));
#19691=CARTESIAN_POINT('Ctrl Pts',(97.2603393637083,1.79519853552882,1.27865843823917));
#19692=CARTESIAN_POINT('Ctrl Pts',(97.2620080303289,1.77766690001696,1.30305047891928));
#19693=CARTESIAN_POINT('Ctrl Pts',(97.263166725419,1.76541353855386,1.31960415797661));
#19694=CARTESIAN_POINT('Ctrl Pts',(97.2709099317092,1.6828667606546,1.4279129869599));
#19695=CARTESIAN_POINT('Ctrl Pts',(97.2778480086945,1.60568520366668,1.5141819456416));
#19696=CARTESIAN_POINT('Ctrl Pts',(97.2915767065824,1.44041902272347,1.67199443470786));
#19697=CARTESIAN_POINT('Ctrl Pts',(97.2983454381227,1.35285361347675,1.74360639672075));
#19698=CARTESIAN_POINT('Ctrl Pts',(97.3075023826572,1.22332316842911,1.83387963628771));
#19699=CARTESIAN_POINT('Ctrl Pts',(97.3100730656522,1.18568920656398,1.85843363857608));
#19700=CARTESIAN_POINT('Ctrl Pts',(97.3144987477146,1.11859715317977,1.89933904364343));
#19701=CARTESIAN_POINT('Ctrl Pts',(97.3163709276377,1.08946671918313,1.91619697260344));
#19702=CARTESIAN_POINT('Ctrl Pts',(97.3191094371916,1.04574898388846,1.94017725915547));
#19703=CARTESIAN_POINT('Ctrl Pts',(97.3199940472822,1.03145167067706,1.94781575235171));
#19704=CARTESIAN_POINT('Ctrl Pts',(97.32156506603,1.00575029909533,1.96118463513976));
#19705=CARTESIAN_POINT('Ctrl Pts',(97.3222535698145,0.994378393033289,1.96697495110217));
#19706=CARTESIAN_POINT('Ctrl Pts',(97.3237082908929,0.970124217661067,1.97906052477348));
#19707=CARTESIAN_POINT('Ctrl Pts',(97.3244735669585,0.9572294779321,1.98532951881347));
#19708=CARTESIAN_POINT('Ctrl Pts',(97.3265284606674,0.92224640270622,2.00191705413486));
#19709=CARTESIAN_POINT('Ctrl Pts',(97.3278097973551,0.900046213809432,2.01199582363293));
#19710=CARTESIAN_POINT('Ctrl Pts',(97.3346722029672,0.779161736921847,2.06447541421351));
#19711=CARTESIAN_POINT('Ctrl Pts',(97.3400167873889,0.67764152974858,2.09998979031711));
#19712=CARTESIAN_POINT('Ctrl Pts',(97.3520014294974,0.440474355470889,2.16395551373336));
#19713=CARTESIAN_POINT('Ctrl Pts',(97.358541452668,0.303940165817493,2.18731286520492));
#19714=CARTESIAN_POINT('Ctrl Pts',(97.3682155346815,0.110845247889272,2.20190889510372));
#19715=CARTESIAN_POINT('Ctrl Pts',(97.3710429553254,0.0554303166240454,
2.204));
#19716=CARTESIAN_POINT('Ctrl Pts',(97.3739726165667,2.84962952926334E-13,
2.204));
#19717=CARTESIAN_POINT('Origin',(66.9212607628943,0.,0.));
#19718=CARTESIAN_POINT('',(98.2342289786285,-4.90954494829228E-11,2.204));
#19719=CARTESIAN_POINT('',(98.1265335566918,1.10792599586928E-10,2.204));
#19720=CARTESIAN_POINT('',(66.9212607628943,-2.69912154532077E-16,2.204));
#19721=CARTESIAN_POINT('',(98.234131513614,0.00201603627767701,2.20399905814364));
#19722=CARTESIAN_POINT('Ctrl Pts',(98.2342289786285,-4.90954494829228E-11,
2.204));
#19723=CARTESIAN_POINT('Ctrl Pts',(98.2341964771698,0.000672034549184021,
2.20400000000001));
#19724=CARTESIAN_POINT('Ctrl Pts',(98.2341639765587,0.0013440747103176,
2.203999692629));
#19725=CARTESIAN_POINT('Ctrl Pts',(98.234131476736,0.00201612022368431,
2.20399907787169));
#19726=CARTESIAN_POINT('Ctrl Pts',(98.2341314808713,0.00201603471236662,
2.20399907794991));
#19727=CARTESIAN_POINT('Ctrl Pts',(98.2270286940923,0.148890558395576,2.20386472937369));
#19728=CARTESIAN_POINT('Ctrl Pts',(98.2200162894635,0.295367267902672,2.1890492234998));
#19729=CARTESIAN_POINT('Ctrl Pts',(98.2113583876976,0.457622973732756,2.15604922601805));
#19730=CARTESIAN_POINT('Ctrl Pts',(98.2103679273346,0.475934480175369,2.15208117309754));
#19731=CARTESIAN_POINT('Ctrl Pts',(98.2088831959586,0.502962919153579,2.14586236583687));
#19732=CARTESIAN_POINT('Ctrl Pts',(98.2083985523008,0.511720679096874,2.1437907854999));
#19733=CARTESIAN_POINT('Ctrl Pts',(98.2075639974475,0.526684432213262,2.14015430986641));
#19734=CARTESIAN_POINT('Ctrl Pts',(98.2072155996558,0.532896662933989,2.13861593246557));
#19735=CARTESIAN_POINT('Ctrl Pts',(98.2064123666166,0.547138557964507,2.13502320607096));
#19736=CARTESIAN_POINT('Ctrl Pts',(98.2059565152877,0.555163231328493,2.13295064969659));
#19737=CARTESIAN_POINT('Ctrl Pts',(98.2046797457496,0.577485382080972,2.12705093931864));
#19738=CARTESIAN_POINT('Ctrl Pts',(98.2038534904878,0.59175602530952,2.12312501921843));
#19739=CARTESIAN_POINT('Ctrl Pts',(98.198582860931,0.681773656154838,2.09738270870218));
#19740=CARTESIAN_POINT('Ctrl Pts',(98.1939547778149,0.756337961105009,2.07166121677561));
#19741=CARTESIAN_POINT('Ctrl Pts',(98.1842391738421,0.907422718482555,2.01029837012323));
#19742=CARTESIAN_POINT('Ctrl Pts',(98.1791507272464,0.983605511284114,1.97414176607105));
#19743=CARTESIAN_POINT('Ctrl Pts',(98.1687082226919,1.13674177185232,1.89039283539825));
#19744=CARTESIAN_POINT('Ctrl Pts',(98.1633719055042,1.21322135735851,1.84224409854052));
#19745=CARTESIAN_POINT('Ctrl Pts',(98.1550365790212,1.33101780050677,1.75755760689232));
#19746=CARTESIAN_POINT('Ctrl Pts',(98.1519454099199,1.37429313851033,1.72393046208749));
#19747=CARTESIAN_POINT('Ctrl Pts',(98.1478420768162,1.43117574346848,1.67622501018439));
#19748=CARTESIAN_POINT('Ctrl Pts',(98.1467750738386,1.44591254615666,1.66352975224271));
#19749=CARTESIAN_POINT('Ctrl Pts',(98.1449973597383,1.47036678567529,1.64189274862729));
#19750=CARTESIAN_POINT('Ctrl Pts',(98.1442823489422,1.48017520655513,1.63305592401006));
#19751=CARTESIAN_POINT('Ctrl Pts',(98.1428758770113,1.49941151789059,1.61540941231897));
#19752=CARTESIAN_POINT('Ctrl Pts',(98.1421842775774,1.50884260991705,1.60660401395612));
#19753=CARTESIAN_POINT('Ctrl Pts',(98.140504825421,1.53167154123291,1.58491130518202));
#19754=CARTESIAN_POINT('Ctrl Pts',(98.1395208140174,1.54498483002539,1.57193621334693));
#19755=CARTESIAN_POINT('Ctrl Pts',(98.1361524779763,1.59031589444744,1.52662438055568));
#19756=CARTESIAN_POINT('Ctrl Pts',(98.1338045142788,1.62149641931428,1.49346455484011));
#19757=CARTESIAN_POINT('Ctrl Pts',(98.1231149061195,1.76083472979661,1.3357687069836));
#19758=CARTESIAN_POINT('Ctrl Pts',(98.1152950718779,1.85581961493352,1.2003133039549));
#19759=CARTESIAN_POINT('Ctrl Pts',(98.1028316747418,1.97847465183779,0.975483312113148));
#19760=CARTESIAN_POINT('Ctrl Pts',(98.0983318461788,2.01712870580203,0.89281487377718));
#19761=CARTESIAN_POINT('Ctrl Pts',(98.092516249203,2.05802197242458,0.789035504941786));
#19762=CARTESIAN_POINT('Ctrl Pts',(98.0914410903269,2.06523081027701,0.769969550612961));
#19763=CARTESIAN_POINT('Ctrl Pts',(98.0898535410641,2.07534450936516,0.742056461935275));
#19764=CARTESIAN_POINT('Ctrl Pts',(98.0893528047449,2.07845957260975,0.733286045112361));
#19765=CARTESIAN_POINT('Ctrl Pts',(98.0884675542279,2.08383319289476,0.71784732992193));
#19766=CARTESIAN_POINT('Ctrl Pts',(98.0880844359571,2.08611548391388,0.711187564045846));
#19767=CARTESIAN_POINT('Ctrl Pts',(98.0872439175435,2.09102787352245,0.696625999352936));
#19768=CARTESIAN_POINT('Ctrl Pts',(98.0867858150148,2.09364506978451,0.688720311820022));
#19769=CARTESIAN_POINT('Ctrl Pts',(98.0854968197394,2.10084403031279,0.666554354979852));
#19770=CARTESIAN_POINT('Ctrl Pts',(98.0846604318679,2.10532523715449,0.652262193102311));
#19771=CARTESIAN_POINT('Ctrl Pts',(98.0789547604889,2.13465093323776,0.555280303672436));
#19772=CARTESIAN_POINT('Ctrl Pts',(98.0738653228241,2.1547613324381,0.471244809066967));
#19773=CARTESIAN_POINT('Ctrl Pts',(98.0668797545049,2.17525681082835,0.356106148807667));
#19774=CARTESIAN_POINT('Ctrl Pts',(98.0650425495561,2.17999460212193,0.325848556119625));
#19775=CARTESIAN_POINT('Ctrl Pts',(98.0576172487835,2.1965704567011,0.203334049657282));
#19776=CARTESIAN_POINT('Ctrl Pts',(98.0520248087108,2.20319442002864,0.110464420699547));
#19777=CARTESIAN_POINT('Ctrl Pts',(98.0411877751727,2.20465262720684,-0.0736963547790665));
#19778=CARTESIAN_POINT('Ctrl Pts',(98.0359488171857,2.19971949004917,-0.164808255245748));
#19779=CARTESIAN_POINT('Ctrl Pts',(98.0296228387593,2.18652619401912,-0.277911088664449));
#19780=CARTESIAN_POINT('Ctrl Pts',(98.0283725011856,2.18354760031787,-0.300418544628712));
#19781=CARTESIAN_POINT('Ctrl Pts',(98.0263749497759,2.17818727087814,-0.33661412960573));
#19782=CARTESIAN_POINT('Ctrl Pts',(98.0256209361727,2.17602300308047,-0.350332358966968));
#19783=CARTESIAN_POINT('Ctrl Pts',(98.0241851999535,2.17163141200565,-0.37655586892633));
#19784=CARTESIAN_POINT('Ctrl Pts',(98.0235028338366,2.16942537170103,-0.389064105271915));
#19785=CARTESIAN_POINT('Ctrl Pts',(98.0219506110023,2.16413501261388,-0.417615265017852));
#19786=CARTESIAN_POINT('Ctrl Pts',(98.0210830327286,2.16098018493305,-0.433644465119808));
#19787=CARTESIAN_POINT('Ctrl Pts',(98.0187776223919,2.15206735768126,-0.476413901197065));
#19788=CARTESIAN_POINT('Ctrl Pts',(98.0173499567301,2.14598922882145,-0.503084916011854));
#19789=CARTESIAN_POINT('Ctrl Pts',(98.0074517682779,2.09995193375955,-0.689048108089269));
#19790=CARTESIAN_POINT('Ctrl Pts',(97.9995695902075,2.04279620316474,-0.84354845259458));
#19791=CARTESIAN_POINT('Ctrl Pts',(97.985680886833,1.91382144496436,-1.09999389293011));
#19792=CARTESIAN_POINT('Ctrl Pts',(97.9797091064346,1.84957233960686,-1.20489594053515));
#19793=CARTESIAN_POINT('Ctrl Pts',(97.9724274054087,1.76767962971349,-1.31649890443952));
#19794=CARTESIAN_POINT('Ctrl Pts',(97.9715968276835,1.75829272715278,-1.32900989338143));
#19795=CARTESIAN_POINT('Ctrl Pts',(97.9703077986237,1.74367481469261,-1.34806688502856));
#19796=CARTESIAN_POINT('Ctrl Pts',(97.9698556485647,1.73853812279116,-1.35468497327124));
#19797=CARTESIAN_POINT('Ctrl Pts',(97.9690152779514,1.72897786039534,-1.36685843713993));
#19798=CARTESIAN_POINT('Ctrl Pts',(97.9686277979266,1.72456502976831,-1.37242190400762));
#19799=CARTESIAN_POINT('Ctrl Pts',(97.9677382804848,1.71442327904374,-1.38508194719722));
#19800=CARTESIAN_POINT('Ctrl Pts',(97.9672350449682,1.70867713688196,-1.39216436386839));
#19801=CARTESIAN_POINT('Ctrl Pts',(97.9656246944401,1.69025596913404,-1.41458355414198));
#19802=CARTESIAN_POINT('Ctrl Pts',(97.964506739891,1.67741748605676,-1.42978403745721));
#19803=CARTESIAN_POINT('Ctrl Pts',(97.9556166213358,1.57477120516605,-1.54802946627635));
#19804=CARTESIAN_POINT('Ctrl Pts',(97.9473453343271,1.47576520690954,-1.64268430517698));
#19805=CARTESIAN_POINT('Ctrl Pts',(97.9329622909477,1.28792582248012,-1.79149846521664));
#19806=CARTESIAN_POINT('Ctrl Pts',(97.9268343703174,1.20282376070939,-1.84971295152347));
#19807=CARTESIAN_POINT('Ctrl Pts',(97.9174595881689,1.06254300646766,-1.9318821484809));
#19808=CARTESIAN_POINT('Ctrl Pts',(97.9140888186555,1.00992647470567,-1.95990197216647));
#19809=CARTESIAN_POINT('Ctrl Pts',(97.9096896484184,0.938274529594791,-1.99440575040151));
#19810=CARTESIAN_POINT('Ctrl Pts',(97.9085953453793,0.92019692882798,-2.00281078467114));
#19811=CARTESIAN_POINT('Ctrl Pts',(97.9067850201258,0.889871725667172,-2.01641295755481));
#19812=CARTESIAN_POINT('Ctrl Pts',(97.9060643501978,0.877686894505272,-2.02174643059638));
#19813=CARTESIAN_POINT('Ctrl Pts',(97.904656052782,0.853657363335134,-2.03200631040321));
#19814=CARTESIAN_POINT('Ctrl Pts',(97.903968189957,0.841816473414707,-2.03694024806575));
#19815=CARTESIAN_POINT('Ctrl Pts',(97.9023136846849,0.813088726235343,-2.04861741961784));
#19816=CARTESIAN_POINT('Ctrl Pts',(97.9013506072553,0.796160039317716,-2.05525565977577));
#19817=CARTESIAN_POINT('Ctrl Pts',(97.8981383396155,0.739025604811676,-2.07684788467916));
#19818=CARTESIAN_POINT('Ctrl Pts',(97.8959209736701,0.698464758573888,-2.09083793629388));
#19819=CARTESIAN_POINT('Ctrl Pts',(97.8852335567862,0.4981548369933,-2.15344748637794));
#19820=CARTESIAN_POINT('Ctrl Pts',(97.8773131338468,0.33365129859371,-2.18498808745691));
#19821=CARTESIAN_POINT('Ctrl Pts',(97.8646918669091,0.074908841732648,-2.20466867155915));
#19822=CARTESIAN_POINT('Ctrl Pts',(97.860130490703,-0.0176833789133627,
-2.20586931871442));
#19823=CARTESIAN_POINT('Ctrl Pts',(97.8542395149129,-0.130560089371308,
-2.20022522979623));
#19824=CARTESIAN_POINT('Ctrl Pts',(97.8531574100386,-0.151036713195516,
-2.19891447093399));
#19825=CARTESIAN_POINT('Ctrl Pts',(97.8515614550278,-0.18079487221796,-2.19659197339418));
#19826=CARTESIAN_POINT('Ctrl Pts',(97.8510594333584,-0.190093553904758,
-2.19580680338551));
#19827=CARTESIAN_POINT('Ctrl Pts',(97.8501693191745,-0.206464079299201,
-2.19431973175649));
#19828=CARTESIAN_POINT('Ctrl Pts',(97.8497826040625,-0.213537913102688,
-2.1936426462477));
#19829=CARTESIAN_POINT('Ctrl Pts',(97.8489378660569,-0.22890481819751,-2.19209673804386));
#19830=CARTESIAN_POINT('Ctrl Pts',(97.8484791710552,-0.237196150659646,
-2.191215075285));
#19831=CARTESIAN_POINT('Ctrl Pts',(97.8471869515582,-0.260413701318517,
-2.18861290690973));
#19832=CARTESIAN_POINT('Ctrl Pts',(97.8463478899117,-0.275327346641447,
-2.18678681608414));
#19833=CARTESIAN_POINT('Ctrl Pts',(97.8405323299162,-0.377688835355098,
-2.17318954809243));
#19834=CARTESIAN_POINT('Ctrl Pts',(97.8353260417339,-0.464372628511995,
-2.15632948391451));
#19835=CARTESIAN_POINT('Ctrl Pts',(97.8285151252054,-0.574729665139916,
-2.12790139447152));
#19836=CARTESIAN_POINT('Ctrl Pts',(97.8269713737107,-0.599541039995519,
-2.12104433057611));
#19837=CARTESIAN_POINT('Ctrl Pts',(97.8201369658291,-0.708698511495932,
-2.08880833509606));
#19838=CARTESIAN_POINT('Ctrl Pts',(97.8148368380289,-0.791602650909097,
-2.05882010483688));
#19839=CARTESIAN_POINT('Ctrl Pts',(97.8057848284572,-0.932370723110672,
-1.99813728621645));
#19840=CARTESIAN_POINT('Ctrl Pts',(97.8019916761946,-0.991077973277591,
-1.96967847846661));
#19841=CARTESIAN_POINT('Ctrl Pts',(97.7957676258696,-1.08726428822042,-1.91766015675686));
#19842=CARTESIAN_POINT('Ctrl Pts',(97.793293708354,-1.1254502014196,-1.89550160820989));
#19843=CARTESIAN_POINT('Ctrl Pts',(97.7898749869974,-1.17813887378265,-1.86277337311782));
#19844=CARTESIAN_POINT('Ctrl Pts',(97.7888960578268,-1.1932156894578,-1.85315196100542));
#19845=CARTESIAN_POINT('Ctrl Pts',(97.7872226316068,-1.21896499102532,-1.83627525642573));
#19846=CARTESIAN_POINT('Ctrl Pts',(97.786524905561,-1.22969377704381,-1.82910789493519));
#19847=CARTESIAN_POINT('Ctrl Pts',(97.7851944842947,-1.25013398266664,-1.81519168700584));
#19848=CARTESIAN_POINT('Ctrl Pts',(97.7845612457082,-1.2598552059718,-1.80845810089318));
#19849=CARTESIAN_POINT('Ctrl Pts',(97.7829111735733,-1.28516184569802,-1.79062589401322));
#19850=CARTESIAN_POINT('Ctrl Pts',(97.7818991750059,-1.30065793982881,-1.77940187038127));
#19851=CARTESIAN_POINT('Ctrl Pts',(97.7783272911256,-1.35523255419602,-1.73877887372259));
#19852=CARTESIAN_POINT('Ctrl Pts',(97.7758100770669,-1.39347787274922,-1.70828192034592));
#19853=CARTESIAN_POINT('Ctrl Pts',(97.7651787266073,-1.55318945527303,-1.57199140756423));
#19854=CARTESIAN_POINT('Ctrl Pts',(97.7575419554663,-1.66386874066126,-1.45433713338));
#19855=CARTESIAN_POINT('Ctrl Pts',(97.7452968975513,-1.81517521581479,-1.25337333055694));
#19856=CARTESIAN_POINT('Ctrl Pts',(97.7408284892806,-1.86509870164113,-1.1777986378688));
#19857=CARTESIAN_POINT('Ctrl Pts',(97.7350513625245,-1.92036407056261,-1.08177191335072));
#19858=CARTESIAN_POINT('Ctrl Pts',(97.733979776966,-1.93025238694271,-1.06402739665507));
#19859=CARTESIAN_POINT('Ctrl Pts',(97.7323965533995,-1.94430544193075,-1.03796856302757));
#19860=CARTESIAN_POINT('Ctrl Pts',(97.7318964802183,-1.94866533144386,-1.02976007355393));
#19861=CARTESIAN_POINT('Ctrl Pts',(97.7310084897439,-1.95626524409029,-1.01523039139992));
#19862=CARTESIAN_POINT('Ctrl Pts',(97.730621925645,-1.95952681417951,-1.00892076787065));
#19863=CARTESIAN_POINT('Ctrl Pts',(97.7297759055652,-1.96656254990003,-0.99514706902523));
#19864=CARTESIAN_POINT('Ctrl Pts',(97.7293157594011,-1.97032469410964,-0.987677349495753));
#19865=CARTESIAN_POINT('Ctrl Pts',(97.7280156296397,-1.98077735356021,-0.966626242502675));
#19866=CARTESIAN_POINT('Ctrl Pts',(97.7271700051735,-1.98737044889088,-0.952997319026223));
#19867=CARTESIAN_POINT('Ctrl Pts',(97.7209709952405,-2.03426931223523,-0.853446790372424));
#19868=CARTESIAN_POINT('Ctrl Pts',(97.7153522306968,-2.06912490360362,-0.765076349048055));
#19869=CARTESIAN_POINT('Ctrl Pts',(97.7040550325685,-2.12689312019023,-0.585441296467138));
#19870=CARTESIAN_POINT('Ctrl Pts',(97.6983901197412,-2.14988200016011,-0.494392652519302));
#19871=CARTESIAN_POINT('Ctrl Pts',(97.6862797948423,-2.18710615492108,-0.293811698490952));
#19872=CARTESIAN_POINT('Ctrl Pts',(97.6798914887765,-2.19906131384067,-0.184101963131649));
#19873=CARTESIAN_POINT('Ctrl Pts',(97.672438936157,-2.20355541761292,-0.0502266972342789));
#19874=CARTESIAN_POINT('Ctrl Pts',(97.6711304045857,-2.20396851336426,-0.0264963000790465));
#19875=CARTESIAN_POINT('Ctrl Pts',(97.6690630214664,-2.20401595614999,0.0113455247942131));
#19876=CARTESIAN_POINT('Ctrl Pts',(97.668296493327,-2.20389817088405,0.0254542980631437));
#19877=CARTESIAN_POINT('Ctrl Pts',(97.6668508535382,-2.20341788975674,0.0522069995418382));
#19878=CARTESIAN_POINT('Ctrl Pts',(97.6661709378527,-2.20308201225533,0.0648507843412206));
#19879=CARTESIAN_POINT('Ctrl Pts',(97.6646285693699,-2.20206818246986,0.0936682546476339));
#19880=CARTESIAN_POINT('Ctrl Pts',(97.6637683214156,-2.20132084550619,0.109838864833555));
#19881=CARTESIAN_POINT('Ctrl Pts',(97.6615287678349,-2.19889633229499,0.152179219122569));
#19882=CARTESIAN_POINT('Ctrl Pts',(97.660158465896,-2.1969301332216,0.178330200876878));
#19883=CARTESIAN_POINT('Ctrl Pts',(97.6496653700656,-2.17812058866877,0.380234802495082));
#19884=CARTESIAN_POINT('Ctrl Pts',(97.6412413281975,-2.14068174594103,0.553420249749476));
#19885=CARTESIAN_POINT('Ctrl Pts',(97.6272034225631,-2.04603638624366,0.82712017748541));
#19886=CARTESIAN_POINT('Ctrl Pts',(97.6216698916669,-2.00093609665839,0.930935918138566));
#19887=CARTESIAN_POINT('Ctrl Pts',(97.6149133865938,-1.94089879706604,1.04439633208269));
#19888=CARTESIAN_POINT('Ctrl Pts',(97.6140975160856,-1.93357474963509,1.05789437103285));
#19889=CARTESIAN_POINT('Ctrl Pts',(97.6128265871947,-1.9220672861888,1.07858357841687));
#19890=CARTESIAN_POINT('Ctrl Pts',(97.6123775565714,-1.91798306868425,1.08582969746773));
#19891=CARTESIAN_POINT('Ctrl Pts',(97.6115398283888,-1.9103321749431,1.09922587514199));
#19892=CARTESIAN_POINT('Ctrl Pts',(97.6111518290531,-1.90677664794049,1.10538199435749));
#19893=CARTESIAN_POINT('Ctrl Pts',(97.6102570685265,-1.89854935397514,1.11946910413472));
#19894=CARTESIAN_POINT('Ctrl Pts',(97.6097490550458,-1.89385763210844,1.12738812646058));
#19895=CARTESIAN_POINT('Ctrl Pts',(97.6081077340414,-1.87862825246728,1.15273001498408));
#19896=CARTESIAN_POINT('Ctrl Pts',(97.6069630142231,-1.86789899788994,1.17003584206345));
#19897=CARTESIAN_POINT('Ctrl Pts',(97.5985365871519,-1.78801171501633,1.29499078590272));
#19898=CARTESIAN_POINT('Ctrl Pts',(97.5908194350833,-1.70984018335472,1.39657757580317));
#19899=CARTESIAN_POINT('Ctrl Pts',(97.5766110097006,-1.54982539267471,1.57081466211898));
#19900=CARTESIAN_POINT('Ctrl Pts',(97.5701280359214,-1.47052337993432,1.64529091183963));
#19901=CARTESIAN_POINT('Ctrl Pts',(97.5614767918747,-1.35404517101395,1.73950329386397));
#19902=CARTESIAN_POINT('Ctrl Pts',(97.5591302115008,-1.32132406607491,1.76448662523567));
#19903=CARTESIAN_POINT('Ctrl Pts',(97.5550520758503,-1.26241636581344,1.80690583681462));
#19904=CARTESIAN_POINT('Ctrl Pts',(97.5533067126958,-1.23652100993213,1.82472455993171));
#19905=CARTESIAN_POINT('Ctrl Pts',(97.5507213058967,-1.19713865766299,1.85060023894928));
#19906=CARTESIAN_POINT('Ctrl Pts',(97.5498656613931,-1.18393303038082,1.85907633183826));
#19907=CARTESIAN_POINT('Ctrl Pts',(97.5483386098135,-1.16005916731179,1.87404231852859));
#19908=CARTESIAN_POINT('Ctrl Pts',(97.5476653090696,-1.14942426456643,1.88058388599666));
#19909=CARTESIAN_POINT('Ctrl Pts',(97.5462236315818,-1.12642179970852,1.89446476032377));
#19910=CARTESIAN_POINT('Ctrl Pts',(97.545456369417,-1.11403679087701,1.90177412984097));
#19911=CARTESIAN_POINT('Ctrl Pts',(97.5434010150872,-1.08048113071215,1.92113767792088));
#19912=CARTESIAN_POINT('Ctrl Pts',(97.5421211534776,-1.05918039966124,1.93296311254612));
#19913=CARTESIAN_POINT('Ctrl Pts',(97.533905054495,-0.919925260327332,2.00727952436785));
#19914=CARTESIAN_POINT('Ctrl Pts',(97.5273511557389,-0.796693711034568,
2.05930034086876));
#19915=CARTESIAN_POINT('Ctrl Pts',(97.5153898051674,-0.561415042203283,
2.13431467012366));
#19916=CARTESIAN_POINT('Ctrl Pts',(97.5099687605223,-0.450836392335652,
2.16037725357833));
#19917=CARTESIAN_POINT('Ctrl Pts',(97.5015869948797,-0.285289435514515,
2.18612742443964));
#19918=CARTESIAN_POINT('Ctrl Pts',(97.498823830923,-0.231544647041384,2.19247106995145));
#19919=CARTESIAN_POINT('Ctrl Pts',(97.4952641590509,-0.16445539315729,2.19789558458065));
#19920=CARTESIAN_POINT('Ctrl Pts',(97.4945596228558,-0.151276623791019,
2.19884195499415));
#19921=CARTESIAN_POINT('Ctrl Pts',(97.4934260549857,-0.130250957173296,
2.20016190047417));
#19922=CARTESIAN_POINT('Ctrl Pts',(97.4930011542303,-0.122408995833271,
2.2006121271039));
#19923=CARTESIAN_POINT('Ctrl Pts',(97.4921802432662,-0.107338378271166,
2.20139656512652));
#19924=CARTESIAN_POINT('Ctrl Pts',(97.4917845794784,-0.100110263445036,
2.20173710828022));
#19925=CARTESIAN_POINT('Ctrl Pts',(97.4909109000873,-0.0842245746124726,
2.20240715666773));
#19926=CARTESIAN_POINT('Ctrl Pts',(97.4904320531775,-0.0755664671458614,
2.20272121854087));
#19927=CARTESIAN_POINT('Ctrl Pts',(97.4887213868041,-0.0447972006561152,
2.20365571262157));
#19928=CARTESIAN_POINT('Ctrl Pts',(97.4874753344573,-0.0226795084516347,
2.2039942950221));
#19929=CARTESIAN_POINT('Ctrl Pts',(97.4862047194752,-0.000374238760942893,
2.20399997617039));
#19930=CARTESIAN_POINT('Ctrl Pts',(97.4861940592604,-0.000187119293676933,
2.204));
#19931=CARTESIAN_POINT('Ctrl Pts',(97.4861833980632,7.30595079061364E-14,
2.204));
#19932=CARTESIAN_POINT('',(98.1264124210279,0.00202521791090988,2.20399901632153));
#19933=CARTESIAN_POINT('Ctrl Pts',(97.3739726165667,2.84962952926334E-13,
2.204));
#19934=CARTESIAN_POINT('Ctrl Pts',(97.3739819747949,-0.000177061274001931,
2.204));
#19935=CARTESIAN_POINT('Ctrl Pts',(97.3739913340681,-0.000354122705178335,
2.20399997866332));
#19936=CARTESIAN_POINT('Ctrl Pts',(97.3747093145248,-0.0139355771281671,
2.20399670540768));
#19937=CARTESIAN_POINT('Ctrl Pts',(97.3754238522532,-0.0273393297549546,
2.2038711897423));
#19938=CARTESIAN_POINT('Ctrl Pts',(97.3765724525169,-0.0486859079455517,
2.20347653248173));
#19939=CARTESIAN_POINT('Ctrl Pts',(97.3770022540842,-0.0566300679190517,
2.20328667634892));
#19940=CARTESIAN_POINT('Ctrl Pts',(97.3778319623752,-0.0718771134803473,
2.20283977582093));
#19941=CARTESIAN_POINT('Ctrl Pts',(97.3782315074757,-0.0791799748172588,
2.20258936781612));
#19942=CARTESIAN_POINT('Ctrl Pts',(97.3792021658589,-0.0968303197220333,
2.20189626377793));
#19943=CARTESIAN_POINT('Ctrl Pts',(97.3797752608472,-0.107176132191411,
2.20141693806801));
#19944=CARTESIAN_POINT('Ctrl Pts',(97.3818185428568,-0.143814463421693,
2.19946058781237));
#19945=CARTESIAN_POINT('Ctrl Pts',(97.3833085595131,-0.170082525029899,
2.19758533101828));
#19946=CARTESIAN_POINT('Ctrl Pts',(97.3871133075049,-0.236228120220814,
2.19167025761626));
#19947=CARTESIAN_POINT('Ctrl Pts',(97.3894517636776,-0.276040118186444,
2.18701252439136));
#19948=CARTESIAN_POINT('Ctrl Pts',(97.4014905943729,-0.477977128922408,
2.15778568355572));
#19949=CARTESIAN_POINT('Ctrl Pts',(97.4115163510578,-0.63712951839179,2.11626412101436));
#19950=CARTESIAN_POINT('Ctrl Pts',(97.4258180588067,-0.865220482945043,
2.02866096924363));
#19951=CARTESIAN_POINT('Ctrl Pts',(97.4304173668542,-0.938600866347626,
1.99577114704289));
#19952=CARTESIAN_POINT('Ctrl Pts',(97.4361450241761,-1.03023623264672,1.94852412254093));
#19953=CARTESIAN_POINT('Ctrl Pts',(97.4373972753262,-1.05028284493818,1.93779228802723));
#19954=CARTESIAN_POINT('Ctrl Pts',(97.4394020226731,-1.08238611266425,1.91996142736631));
#19955=CARTESIAN_POINT('Ctrl Pts',(97.4401612937447,-1.09454715501363,1.91305465619415));
#19956=CARTESIAN_POINT('Ctrl Pts',(97.4416098387214,-1.11774851771764,1.89958395264468));
#19957=CARTESIAN_POINT('Ctrl Pts',(97.4422997358875,-1.12879878081432,1.89303836836737));
#19958=CARTESIAN_POINT('Ctrl Pts',(97.4438884091429,-1.1542404510714,1.87766609828384));
#19959=CARTESIAN_POINT('Ctrl Pts',(97.444784596387,-1.16858901406738,1.86876984487803));
#19960=CARTESIAN_POINT('Ctrl Pts',(97.4476458532578,-1.21436968482697,1.83965188538493));
#19961=CARTESIAN_POINT('Ctrl Pts',(97.4495874108625,-1.24539095433056,1.81879475893508));
#19962=CARTESIAN_POINT('Ctrl Pts',(97.4574885874725,-1.37109110770589,1.72955563093991));
#19963=CARTESIAN_POINT('Ctrl Pts',(97.4631965762121,-1.46079592978947,1.65448841864075));
#19964=CARTESIAN_POINT('Ctrl Pts',(97.4758452255033,-1.64725260362292,1.47141414430502));
#19965=CARTESIAN_POINT('Ctrl Pts',(97.482724459768,-1.74015249385944,1.36027987710566));
#19966=CARTESIAN_POINT('Ctrl Pts',(97.4914874927377,-1.83556992010327,1.22021460888507));
#19967=CARTESIAN_POINT('Ctrl Pts',(97.4927973148451,-1.84928795568172,1.19932254933254));
#19968=CARTESIAN_POINT('Ctrl Pts',(97.4946853321914,-1.86823069530785,1.16937554361205));
#19969=CARTESIAN_POINT('Ctrl Pts',(97.4952456021945,-1.87375126651548,1.16050905870864));
#19970=CARTESIAN_POINT('Ctrl Pts',(97.4962016895332,-1.88299679633206,1.14542203186685));
#19971=CARTESIAN_POINT('Ctrl Pts',(97.4965954006271,-1.88675453626141,1.13922161372622));
#19972=CARTESIAN_POINT('Ctrl Pts',(97.497421797826,-1.89453711216455,1.12623592895191));
#19973=CARTESIAN_POINT('Ctrl Pts',(97.4978548202945,-1.89855618027697,1.11944748128097));
#19974=CARTESIAN_POINT('Ctrl Pts',(97.4990152505106,-1.90917334749632,1.10129281084416));
#19975=CARTESIAN_POINT('Ctrl Pts',(97.4997466340787,-1.91570627171185,1.08988907198684));
#19976=CARTESIAN_POINT('Ctrl Pts',(97.5034005576062,-1.94758746315883,1.03306560912353));
#19977=CARTESIAN_POINT('Ctrl Pts',(97.5064039727004,-1.97142267587486,0.986819797132146));
#19978=CARTESIAN_POINT('Ctrl Pts',(97.516479817641,-2.04460298224934,0.831578753127164));
#19979=CARTESIAN_POINT('Ctrl Pts',(97.5237387560793,-2.08671379769918,0.719409118755392));
#19980=CARTESIAN_POINT('Ctrl Pts',(97.5386095833968,-2.15495791891663,0.480081561977351));
#19981=CARTESIAN_POINT('Ctrl Pts',(97.5461687191451,-2.17940286109702,0.352893433862224));
#19982=CARTESIAN_POINT('Ctrl Pts',(97.5547399703849,-2.19505632379293,0.199865057164176));
#19983=CARTESIAN_POINT('Ctrl Pts',(97.5560948390168,-2.1971458193073,0.175409871931398));
#19984=CARTESIAN_POINT('Ctrl Pts',(97.5582303958799,-2.19982007954713,0.136448356161442));
#19985=CARTESIAN_POINT('Ctrl Pts',(97.5590193373013,-2.20067071885515,0.121962853453563));
#19986=CARTESIAN_POINT('Ctrl Pts',(97.5604857631126,-2.20199335039197,0.0948704659505365));
#19987=CARTESIAN_POINT('Ctrl Pts',(97.5611643136169,-2.20250027086464,0.0822659498780257));
#19988=CARTESIAN_POINT('Ctrl Pts',(97.562689370637,-2.20340079092127,0.0537872920686311));
#19989=CARTESIAN_POINT('Ctrl Pts',(97.563533864746,-2.203731116609,0.0379117633153341));
#19990=CARTESIAN_POINT('Ctrl Pts',(97.5660597055858,-2.20420886298624,-0.00987401067489685));
#19991=CARTESIAN_POINT('Ctrl Pts',(97.5677248169345,-2.20383490307266,-0.041785924652601));
#19992=CARTESIAN_POINT('Ctrl Pts',(97.5715305317536,-2.20136787091285,-0.115541767656108));
#19993=CARTESIAN_POINT('Ctrl Pts',(97.5736561849177,-2.19877453792642,-0.157356898562891));
#19994=CARTESIAN_POINT('Ctrl Pts',(97.5813522913052,-2.18489850743498,-0.310353805301846));
#19995=CARTESIAN_POINT('Ctrl Pts',(97.5867359227622,-2.16635796577845,-0.420708531048811));
#19996=CARTESIAN_POINT('Ctrl Pts',(97.5980787429663,-2.11002410553565,-0.648470812702674));
#19997=CARTESIAN_POINT('Ctrl Pts',(97.6040241653249,-2.07059829559113,-0.765070218177005));
#19998=CARTESIAN_POINT('Ctrl Pts',(97.611502212167,-2.01344792055741,-0.89669930338991));
#19999=CARTESIAN_POINT('Ctrl Pts',(97.6125907346971,-2.00496095628523,-0.915518253611297));
#20000=CARTESIAN_POINT('Ctrl Pts',(97.6141920526109,-1.99226499833944,-0.942646726437807));
#20001=CARTESIAN_POINT('Ctrl Pts',(97.6146928292216,-1.98826546823607,-0.951053676704099));
#20002=CARTESIAN_POINT('Ctrl Pts',(97.6155857691474,-1.98108600146899,-0.96590157376129));
#20003=CARTESIAN_POINT('Ctrl Pts',(97.615976612355,-1.97792767295364,-0.972352669846697));
#20004=CARTESIAN_POINT('Ctrl Pts',(97.6168290536901,-1.9710060005592,-0.986317371540986));
#20005=CARTESIAN_POINT('Ctrl Pts',(97.6172913221002,-1.96723126175271,-0.993824818377816));
#20006=CARTESIAN_POINT('Ctrl Pts',(97.6186146263424,-1.95636229517063,-1.0151371698018));
#20007=CARTESIAN_POINT('Ctrl Pts',(97.6194816960089,-1.94916518215492,-1.02888870549905));
#20008=CARTESIAN_POINT('Ctrl Pts',(97.6270775724272,-1.88540415336963,-1.14764671996824));
#20009=CARTESIAN_POINT('Ctrl Pts',(97.6342216465019,-1.82055253913967,-1.24796841965663));
#20010=CARTESIAN_POINT('Ctrl Pts',(97.6515000574071,-1.6453413775444,-1.47608329081852));
#20011=CARTESIAN_POINT('Ctrl Pts',(97.6615598903468,-1.52778712644834,-1.5974523571444));
#20012=CARTESIAN_POINT('Ctrl Pts',(97.6725282191723,-1.37658453976377,-1.72144285152621));
#20013=CARTESIAN_POINT('Ctrl Pts',(97.6740332760261,-1.35531239180769,-1.73824017300327));
#20014=CARTESIAN_POINT('Ctrl Pts',(97.6764213586757,-1.32071964089144,-1.76453475785449));
#20015=CARTESIAN_POINT('Ctrl Pts',(97.6773141728215,-1.3075942149623,-1.77428314280375));
#20016=CARTESIAN_POINT('Ctrl Pts',(97.6788963189765,-1.28399406147609,-1.79140707668303));
#20017=CARTESIAN_POINT('Ctrl Pts',(97.6795878162813,-1.27356131723132,-1.79883897145362));
#20018=CARTESIAN_POINT('Ctrl Pts',(97.6810336301148,-1.25150259012361,-1.81426467377766));
#20019=CARTESIAN_POINT('Ctrl Pts',(97.6817871706801,-1.23986341774322,-1.82223866648223));
#20020=CARTESIAN_POINT('Ctrl Pts',(97.6837746678168,-1.20879267812378,-1.8430896941797));
#20021=CARTESIAN_POINT('Ctrl Pts',(97.685001282394,-1.1892317571805,-1.85577133342138));
#20022=CARTESIAN_POINT('Ctrl Pts',(97.6913726989779,-1.08568193615649,-1.9205944530065));
#20023=CARTESIAN_POINT('Ctrl Pts',(97.6963187873895,-0.998452872225329,
-1.96735432699394));
#20024=CARTESIAN_POINT('Ctrl Pts',(97.7054405244625,-0.828809683280653,
-2.04409290292321));
#20025=CARTESIAN_POINT('Ctrl Pts',(97.7096322243475,-0.747178790498817,
-2.07532294885835));
#20026=CARTESIAN_POINT('Ctrl Pts',(97.7149424145905,-0.642706693712112,
-2.10832601612228));
#20027=CARTESIAN_POINT('Ctrl Pts',(97.7160227410944,-0.621402576493553,
-2.11470312471845));
#20028=CARTESIAN_POINT('Ctrl Pts',(97.7215623459013,-0.512197546036285,
-2.14559947968191));
#20029=CARTESIAN_POINT('Ctrl Pts',(97.7260940873225,-0.422939459807675,
-2.16496243376399));
#20030=CARTESIAN_POINT('Ctrl Pts',(97.7316955557646,-0.317738287106051,
-2.18102933171089));
#20031=CARTESIAN_POINT('Ctrl Pts',(97.7325021707979,-0.302705094658855,
-2.18316654545788));
#20032=CARTESIAN_POINT('Ctrl Pts',(97.7337691941737,-0.279300215716118,
-2.18624754796377));
#20033=CARTESIAN_POINT('Ctrl Pts',(97.7342238356476,-0.270942900717031,
-2.18729899447918));
#20034=CARTESIAN_POINT('Ctrl Pts',(97.7350710489905,-0.255450885156529,
-2.18915792028793));
#20035=CARTESIAN_POINT('Ctrl Pts',(97.7354628946299,-0.248318029337369,
-2.18997847164813));
#20036=CARTESIAN_POINT('Ctrl Pts',(97.7363744062227,-0.231798906178504,
-2.19179706259628));
#20037=CARTESIAN_POINT('Ctrl Pts',(97.7368954485079,-0.222410132989806,
-2.19276966929072));
#20038=CARTESIAN_POINT('Ctrl Pts',(97.738574920074,-0.192307671445952,-2.19569274271431));
#20039=CARTESIAN_POINT('Ctrl Pts',(97.7397452168932,-0.171573081793909,
-2.1974101743485));
#20040=CARTESIAN_POINT('Ctrl Pts',(97.7463051244522,-0.0564663164599404,
-2.20530535113382));
#20041=CARTESIAN_POINT('Ctrl Pts',(97.7519308003735,0.0381968605775587,
-2.20569676577638));
#20042=CARTESIAN_POINT('Ctrl Pts',(97.7680024877513,0.305716337298381,-2.18957468754965));
#20043=CARTESIAN_POINT('Ctrl Pts',(97.7784470432829,0.477042010246259,-2.15873763621696));
#20044=CARTESIAN_POINT('Ctrl Pts',(97.7903709925441,0.678740718238237,-2.09721813832766));
#20045=CARTESIAN_POINT('Ctrl Pts',(97.7924562422922,0.714208000318182,-2.08540644843603));
#20046=CARTESIAN_POINT('Ctrl Pts',(97.7954306040527,0.765064723374735,-2.06701980380745));
#20047=CARTESIAN_POINT('Ctrl Pts',(97.7963431909379,0.780705368306805,-2.06116327588443));
#20048=CARTESIAN_POINT('Ctrl Pts',(97.7979478943161,0.808267982826948,-2.05048389474645));
#20049=CARTESIAN_POINT('Ctrl Pts',(97.7986423954203,0.820217006189716,-2.04573346436582));
#20050=CARTESIAN_POINT('Ctrl Pts',(97.8000823258282,0.845029278348068,-2.03561679924722));
#20051=CARTESIAN_POINT('Ctrl Pts',(97.8008271088029,0.857884599671815,-2.03023256316219));
#20052=CARTESIAN_POINT('Ctrl Pts',(97.8027642724922,0.891369193842865,-2.01583326608879));
#20053=CARTESIAN_POINT('Ctrl Pts',(97.8039499826605,0.911913199454301,-2.00662332353375));
#20054=CARTESIAN_POINT('Ctrl Pts',(97.8096332006951,1.01053632718484,-1.96058275225846));
#20055=CARTESIAN_POINT('Ctrl Pts',(97.8139823653554,1.08655065568207,-1.91949945101085));
#20056=CARTESIAN_POINT('Ctrl Pts',(97.8230472533561,1.242866426604,-1.82274647232381));
#20057=CARTESIAN_POINT('Ctrl Pts',(97.827726812465,1.32227331827657,-1.76598851095926));
#20058=CARTESIAN_POINT('Ctrl Pts',(97.8334973248447,1.41440353975956,-1.6904281953571));
#20059=CARTESIAN_POINT('Ctrl Pts',(97.8345480103002,1.43094260181277,-1.67645104721564));
#20060=CARTESIAN_POINT('Ctrl Pts',(97.8402631369872,1.51940550957116,-1.59942815015354));
#20061=CARTESIAN_POINT('Ctrl Pts',(97.844998745795,1.58736650273789,-1.53200109219444));
#20062=CARTESIAN_POINT('Ctrl Pts',(97.8508333955863,1.66082609118795,-1.44896687516706));
#20063=CARTESIAN_POINT('Ctrl Pts',(97.8516429821602,1.67080638286428,-1.43744715237542));
#20064=CARTESIAN_POINT('Ctrl Pts',(97.852913696849,1.68612360862381,-1.41939224429187));
#20065=CARTESIAN_POINT('Ctrl Pts',(97.8533690045229,1.69154403011381,-1.41292814966029));
#20066=CARTESIAN_POINT('Ctrl Pts',(97.8542167800272,1.70150785390662,-1.40090633254908));
#20067=CARTESIAN_POINT('Ctrl Pts',(97.8546085124826,1.70606136886374,-1.39535734866986));
#20068=CARTESIAN_POINT('Ctrl Pts',(97.8555188576842,1.7165278840395,-1.38247486971013));
#20069=CARTESIAN_POINT('Ctrl Pts',(97.8560388343347,1.72242103875097,-1.37512563087084));
#20070=CARTESIAN_POINT('Ctrl Pts',(97.8577113915479,1.74111353889568,-1.35150589956215));
#20071=CARTESIAN_POINT('Ctrl Pts',(97.8588757082453,1.75373047864788,-1.33509321654486));
#20072=CARTESIAN_POINT('Ctrl Pts',(97.8653693414449,1.8220663559535,-1.24355859094771));
#20073=CARTESIAN_POINT('Ctrl Pts',(97.8709299076844,1.87318700428819,-1.16513147935897));
#20074=CARTESIAN_POINT('Ctrl Pts',(97.8867432156117,2.00287201345458,-0.935467617968303));
#20075=CARTESIAN_POINT('Ctrl Pts',(97.8970025351573,2.06913352433295,-0.778009283013917));
#20076=CARTESIAN_POINT('Ctrl Pts',(97.9089101026323,2.12766464329978,-0.57639549512677));
#20077=CARTESIAN_POINT('Ctrl Pts',(97.911128043,2.13769142225382,-0.53801883861719));
#20078=CARTESIAN_POINT('Ctrl Pts',(97.9141905327883,2.15028717083408,-0.483874831859102));
#20079=CARTESIAN_POINT('Ctrl Pts',(97.9150627414692,2.15372842600312,-0.468320035671987));
#20080=CARTESIAN_POINT('Ctrl Pts',(97.9165758244013,2.15944057344553,-0.44110484387122));
#20081=CARTESIAN_POINT('Ctrl Pts',(97.9172190702162,2.16178637500982,-0.429460999503841));
#20082=CARTESIAN_POINT('Ctrl Pts',(97.9185652382825,2.16652051057689,-0.404939976325212));
#20083=CARTESIAN_POINT('Ctrl Pts',(97.9192674861822,2.16888843066598,-0.392059297458112));
#20084=CARTESIAN_POINT('Ctrl Pts',(97.9209485458857,2.1743096034208,-0.361016486117458));
#20085=CARTESIAN_POINT('Ctrl Pts',(97.9219237573924,2.17725032399774,-0.342835542204599));
#20086=CARTESIAN_POINT('Ctrl Pts',(97.9253622284056,2.18688298118481,-0.27814800665365));
#20087=CARTESIAN_POINT('Ctrl Pts',(97.9277860402161,2.19231561007408,-0.231465246782524));
#20088=CARTESIAN_POINT('Ctrl Pts',(97.933782719309,2.20221182180191,-0.113753385568278));
#20089=CARTESIAN_POINT('Ctrl Pts',(97.9373011977993,2.20473618571501,-0.0426147235539901));
#20090=CARTESIAN_POINT('Ctrl Pts',(97.9470994666509,2.20213854181846,0.158079084840689));
#20091=CARTESIAN_POINT('Ctrl Pts',(97.9532441747371,2.18904118587867,0.287226901422236));
#20092=CARTESIAN_POINT('Ctrl Pts',(97.9628429614164,2.15263911371629,0.477345821720939));
#20093=CARTESIAN_POINT('Ctrl Pts',(97.9660841463907,2.13786770859342,0.539661483749271));
#20094=CARTESIAN_POINT('Ctrl Pts',(97.9702116916643,2.11651923553246,0.614951569365691));
#20095=CARTESIAN_POINT('Ctrl Pts',(97.9709699493356,2.11249868263135,0.628624213468353));
#20096=CARTESIAN_POINT('Ctrl Pts',(97.9721768363128,2.10595245589098,0.650113617608666));
#20097=CARTESIAN_POINT('Ctrl Pts',(97.9726205400178,2.10351512626195,0.657957119733583));
#20098=CARTESIAN_POINT('Ctrl Pts',(97.9734591143958,2.09885316962731,0.672668933381644));
#20099=CARTESIAN_POINT('Ctrl Pts',(97.9738534128662,2.0966385709436,0.679540152644493));
#20100=CARTESIAN_POINT('Ctrl Pts',(97.9747867315503,2.0913430721749,0.695698131298487));
#20101=CARTESIAN_POINT('Ctrl Pts',(97.9753273557646,2.08823404048459,0.704975403945903));
#20102=CARTESIAN_POINT('Ctrl Pts',(97.9771374536119,2.07768269338171,0.735778061222619));
#20103=CARTESIAN_POINT('Ctrl Pts',(97.978421415721,2.06996873209409,0.757208092262544));
#20104=CARTESIAN_POINT('Ctrl Pts',(97.9815929731626,2.05032155044888,0.809244421388071));
#20105=CARTESIAN_POINT('Ctrl Pts',(97.9834959449694,2.03803365385381,0.839710442971886));
#20106=CARTESIAN_POINT('Ctrl Pts',(97.9916128052812,1.9833383580868,0.967039103553963));
#20107=CARTESIAN_POINT('Ctrl Pts',(97.9980046678959,1.93467110809167,1.0610570907159));
#20108=CARTESIAN_POINT('Ctrl Pts',(98.0124525349574,1.80882924258046,1.266503319181));
#20109=CARTESIAN_POINT('Ctrl Pts',(98.0204332694513,1.7277461150675,1.37506237726276));
#20110=CARTESIAN_POINT('Ctrl Pts',(98.0297899952272,1.6162777451201,1.49874620159978));
#20111=CARTESIAN_POINT('Ctrl Pts',(98.0315272672179,1.59484941166543,1.52152864643736));
#20112=CARTESIAN_POINT('Ctrl Pts',(98.0341199605864,1.56176280023523,1.55523878899609));
#20113=CARTESIAN_POINT('Ctrl Pts',(98.0349905858811,1.55045931789572,1.5665077904208));
#20114=CARTESIAN_POINT('Ctrl Pts',(98.0365462587481,1.52991661443372,1.58654763365523));
#20115=CARTESIAN_POINT('Ctrl Pts',(98.0372332443933,1.52072195880423,1.59536296010865));
#20116=CARTESIAN_POINT('Ctrl Pts',(98.0386946571425,1.50090143053726,1.61403872584742));
#20117=CARTESIAN_POINT('Ctrl Pts',(98.03946803314,1.49025362431559,1.62387507575358));
#20118=CARTESIAN_POINT('Ctrl Pts',(98.0412544372146,1.46529427071392,1.64648003773815));
#20119=CARTESIAN_POINT('Ctrl Pts',(98.042264092706,1.45091144941154,1.65916840947157));
#20120=CARTESIAN_POINT('Ctrl Pts',(98.0473853072951,1.3765816558494,1.72303557593424));
#20121=CARTESIAN_POINT('Ctrl Pts',(98.0513726957121,1.31408327236977,1.77116217553305));
#20122=CARTESIAN_POINT('Ctrl Pts',(98.0610995782985,1.15228120893595,1.88246753794252));
#20123=CARTESIAN_POINT('Ctrl Pts',(98.0667151949082,1.05025210956043,1.94123852519005));
#20124=CARTESIAN_POINT('Ctrl Pts',(98.0775576072156,0.848496048100299,2.0368715533644));
#20125=CARTESIAN_POINT('Ctrl Pts',(98.0827570055827,0.749846741641844,2.07521475979122));
#20126=CARTESIAN_POINT('Ctrl Pts',(98.0891234648794,0.634225338406635,2.11083113510916));
#20127=CARTESIAN_POINT('Ctrl Pts',(98.0899356809216,0.619564464011215,2.11518077475786));
#20128=CARTESIAN_POINT('Ctrl Pts',(98.0912096615471,0.596736938279598,2.12169563880535));
#20129=CARTESIAN_POINT('Ctrl Pts',(98.0916655581014,0.58860082857942,2.12396714122705));
#20130=CARTESIAN_POINT('Ctrl Pts',(98.0925138336167,0.573528460116436,2.12808190947564));
#20131=CARTESIAN_POINT('Ctrl Pts',(98.0929054691384,0.566596024351771,2.12993813256715));
#20132=CARTESIAN_POINT('Ctrl Pts',(98.0938147971304,0.550559011089369,2.13414835666179));
#20133=CARTESIAN_POINT('Ctrl Pts',(98.0943338426409,0.541448338719758,2.13647797152449));
#20134=CARTESIAN_POINT('Ctrl Pts',(98.0960003736084,0.512322359934135,2.14372727160456));
#20135=CARTESIAN_POINT('Ctrl Pts',(98.0971594812687,0.49225338654142,2.14842438928037));
#20136=CARTESIAN_POINT('Ctrl Pts',(98.1073165602986,0.317703723925351,2.18670350473883));
#20137=CARTESIAN_POINT('Ctrl Pts',(98.116963934652,0.16009919970521,2.20385379994168));
#20138=CARTESIAN_POINT('Ctrl Pts',(98.1264124982452,0.00202546956495211,
2.2039990692995));
#20139=CARTESIAN_POINT('Ctrl Pts',(98.126412512956,0.00202522345453538,
2.20399906952566));
#20140=CARTESIAN_POINT('Ctrl Pts',(98.1264528646512,0.00135014273495122,
2.20399968984775));
#20141=CARTESIAN_POINT('Ctrl Pts',(98.1264932125787,0.000675068216677538,
2.20399999999997));
#20142=CARTESIAN_POINT('Ctrl Pts',(98.1265335566918,1.10792599586928E-10,
2.204));
#20143=CARTESIAN_POINT('Origin',(66.9212607628943,0.,0.));
#20144=CARTESIAN_POINT('',(98.9822063149447,-1.02538676663964E-13,2.204));
#20145=CARTESIAN_POINT('',(98.8779717715633,2.72446158072696E-13,2.204));
#20146=CARTESIAN_POINT('',(66.9212607628943,-2.69912154532077E-16,2.204));
#20147=CARTESIAN_POINT('Ctrl Pts',(98.9822063149447,-3.98666500548274E-14,
2.204));
#20148=CARTESIAN_POINT('Ctrl Pts',(98.981345646301,0.0156268070781291,2.204));
#20149=CARTESIAN_POINT('Ctrl Pts',(98.9804901719241,0.0312534512830711,
2.20383380430557));
#20150=CARTESIAN_POINT('Ctrl Pts',(98.9789994524121,0.0586452158235635,
2.20325107173718));
#20151=CARTESIAN_POINT('Ctrl Pts',(98.9783619850133,0.0704110898098772,
2.20290645112726));
#20152=CARTESIAN_POINT('Ctrl Pts',(98.9770292359948,0.0951173970063678,
2.20198466176993));
#20153=CARTESIAN_POINT('Ctrl Pts',(98.9763346021306,0.108056668706093,2.20138763876887));
#20154=CARTESIAN_POINT('Ctrl Pts',(98.9746744975788,0.139124238152045,2.19967958725385));
#20155=CARTESIAN_POINT('Ctrl Pts',(98.9737125075476,0.15724568744745,2.19845847367306));
#20156=CARTESIAN_POINT('Ctrl Pts',(98.9703388404841,0.221186899601767,2.19335513051738));
#20157=CARTESIAN_POINT('Ctrl Pts',(98.9679648478299,0.266899565887535,2.1882630963279));
#20158=CARTESIAN_POINT('Ctrl Pts',(98.9621148908914,0.380855900092877,2.17194476393601));
#20159=CARTESIAN_POINT('Ctrl Pts',(98.958689960001,0.448793922597031,2.15893032782001));
#20160=CARTESIAN_POINT('Ctrl Pts',(98.9486393791114,0.64868511817622,2.11079295139281));
#20161=CARTESIAN_POINT('Ctrl Pts',(98.9421811202234,0.778097826067429,2.06659136720652));
#20162=CARTESIAN_POINT('Ctrl Pts',(98.9323659404591,0.958245081956869,1.98572518355226));
#20163=CARTESIAN_POINT('Ctrl Pts',(98.9292696643993,1.01283829191085,1.95844212634833));
#20164=CARTESIAN_POINT('Ctrl Pts',(98.9253116145229,1.07848270856545,1.92215691482094));
#20165=CARTESIAN_POINT('Ctrl Pts',(98.9245661459634,1.09067521273145,1.9152649211172));
#20166=CARTESIAN_POINT('Ctrl Pts',(98.9233778120495,1.10982167988839,1.90419998759224));
#20167=CARTESIAN_POINT('Ctrl Pts',(98.9229396872366,1.11681991226482,1.90010395325543));
#20168=CARTESIAN_POINT('Ctrl Pts',(98.9221104562412,1.12994661134344,1.89232338368031));
#20169=CARTESIAN_POINT('Ctrl Pts',(98.9217198954444,1.13607993612788,1.88864753365664));
#20170=CARTESIAN_POINT('Ctrl Pts',(98.9207942401351,1.15050262265826,1.87990799493628));
#20171=CARTESIAN_POINT('Ctrl Pts',(98.9202575550501,1.1587765289605,1.87481927204694));
#20172=CARTESIAN_POINT('Ctrl Pts',(98.9184559665107,1.18626981696341,1.8576584832453));
#20173=CARTESIAN_POINT('Ctrl Pts',(98.9171766422279,1.20533573481716,1.84534462994245));
#20174=CARTESIAN_POINT('Ctrl Pts',(98.914014181379,1.25146232681063,1.81453363643569));
#20175=CARTESIAN_POINT('Ctrl Pts',(98.9121156739281,1.27830667619018,1.79572328718996));
#20176=CARTESIAN_POINT('Ctrl Pts',(98.9040056786087,1.3899168975833,1.71374484695117));
#20177=CARTESIAN_POINT('Ctrl Pts',(98.8976156236718,1.47049830152077,1.64512123859726));
#20178=CARTESIAN_POINT('Ctrl Pts',(98.8831264167054,1.64271100952328,1.47566451683766));
#20179=CARTESIAN_POINT('Ctrl Pts',(98.8751039377492,1.73056789160358,1.37157918215866));
#20180=CARTESIAN_POINT('Ctrl Pts',(98.8657254942883,1.826011501533,1.23460903685701));
#20181=CARTESIAN_POINT('Ctrl Pts',(98.8640033250567,1.84320066659682,1.20879647517741));
#20182=CARTESIAN_POINT('Ctrl Pts',(98.8614335808711,1.86832538288025,1.16928453942366));
#20183=CARTESIAN_POINT('Ctrl Pts',(98.8605710468637,1.87666698684141,1.15584908588181));
#20184=CARTESIAN_POINT('Ctrl Pts',(98.8590302624156,1.89139948332306,1.13154011122728));
#20185=CARTESIAN_POINT('Ctrl Pts',(98.8583501039162,1.89784295323834,1.12069940791132));
#20186=CARTESIAN_POINT('Ctrl Pts',(98.8569038443129,1.91141287493478,1.09741623782729));
#20187=CARTESIAN_POINT('Ctrl Pts',(98.8561387651737,1.91851169009653,1.0849582875642));
#20188=CARTESIAN_POINT('Ctrl Pts',(98.8540619190326,1.9375575178991,1.05076261640857));
#20189=CARTESIAN_POINT('Ctrl Pts',(98.8527588727834,1.94926013840631,1.02889075688289));
#20190=CARTESIAN_POINT('Ctrl Pts',(98.8435389266839,2.03019365084294,0.871288906543657));
#20191=CARTESIAN_POINT('Ctrl Pts',(98.83613463766,2.08555588742027,0.728898700749735));
#20192=CARTESIAN_POINT('Ctrl Pts',(98.8221229188616,2.16209616604372,0.449293680386417));
#20193=CARTESIAN_POINT('Ctrl Pts',(98.8155249362084,2.18590674994476,0.313572565464096));
#20194=CARTESIAN_POINT('Ctrl Pts',(98.8073160820554,2.19850571833654,0.15678421013648));
#20195=CARTESIAN_POINT('Ctrl Pts',(98.8062700504793,2.19982644407811,0.137011839118037));
#20196=CARTESIAN_POINT('Ctrl Pts',(98.8047230093116,2.20136464715042,0.108132336014155));
#20197=CARTESIAN_POINT('Ctrl Pts',(98.8042329990128,2.20179258836586,0.0990368805215006));
#20198=CARTESIAN_POINT('Ctrl Pts',(98.8033553374221,2.20245387701171,0.0828452067917682));
#20199=CARTESIAN_POINT('Ctrl Pts',(98.8029689099464,2.20270931368415,0.0757501581093566));
#20200=CARTESIAN_POINT('Ctrl Pts',(98.8021216457691,2.20319176329827,0.0602695470396744));
#20201=CARTESIAN_POINT('Ctrl Pts',(98.8016601014888,2.20340518513577,0.0518840005104393));
#20202=CARTESIAN_POINT('Ctrl Pts',(98.8003279333011,2.2038804213938,0.0278087158807533));
#20203=CARTESIAN_POINT('Ctrl Pts',(98.7994510843705,2.20402254421296,0.0121174398909252));
#20204=CARTESIAN_POINT('Ctrl Pts',(98.7914864586338,2.20379346064208,-0.129170581206396));
#20205=CARTESIAN_POINT('Ctrl Pts',(98.7839409666155,2.19285431426113,-0.254509704886815));
#20206=CARTESIAN_POINT('Ctrl Pts',(98.7667266210241,2.14368442504197,-0.536784875703963));
#20207=CARTESIAN_POINT('Ctrl Pts',(98.7571364971813,2.09877420949042,-0.691869209440657));
#20208=CARTESIAN_POINT('Ctrl Pts',(98.7465535575009,2.02684995392138,-0.866172581729055));
#20209=CARTESIAN_POINT('Ctrl Pts',(98.7450222478677,2.01585928851699,-0.891452243778885));
#20210=CARTESIAN_POINT('Ctrl Pts',(98.7426056485553,1.99757911271466,-0.931430347331973));
#20211=CARTESIAN_POINT('Ctrl Pts',(98.741710075277,1.99059497061757,-0.946264491007038));
#20212=CARTESIAN_POINT('Ctrl Pts',(98.7401304487696,1.97790419169966,-0.972456955810695));
#20213=CARTESIAN_POINT('Ctrl Pts',(98.7394441432905,1.97226366380188,-0.983846315410408));
#20214=CARTESIAN_POINT('Ctrl Pts',(98.7380166524244,1.9602672850207,-1.00755159973478));
#20215=CARTESIAN_POINT('Ctrl Pts',(98.7372761472998,1.95389313765396,-1.01985767316147));
#20216=CARTESIAN_POINT('Ctrl Pts',(98.7353403857479,1.93683527124759,-1.05204297269706));
#20217=CARTESIAN_POINT('Ctrl Pts',(98.734151897556,1.92596142452687,-1.07181991277337));
#20218=CARTESIAN_POINT('Ctrl Pts',(98.7283206558481,1.8706524570423,-1.16885326568765));
#20219=CARTESIAN_POINT('Ctrl Pts',(98.7238369986669,1.82186170150511,-1.24353558743384));
#20220=CARTESIAN_POINT('Ctrl Pts',(98.7147628431058,1.71190018667459,-1.39142688057461));
#20221=CARTESIAN_POINT('Ctrl Pts',(98.7101953754493,1.65023537590249,-1.46403368771191));
#20222=CARTESIAN_POINT('Ctrl Pts',(98.704172438329,1.56377521791967,-1.55340759365115));
#20223=CARTESIAN_POINT('Ctrl Pts',(98.7027548401676,1.54306468148149,-1.5739820312744));
#20224=CARTESIAN_POINT('Ctrl Pts',(98.6970326377795,1.45840561585191,-1.65480750487543));
#20225=CARTESIAN_POINT('Ctrl Pts',(98.6926589087013,1.39129450000088,-1.71161660630004));
#20226=CARTESIAN_POINT('Ctrl Pts',(98.6872432565518,1.30896017292082,-1.77326387038828));
#20227=CARTESIAN_POINT('Ctrl Pts',(98.6864453676975,1.29684857150853,-1.782140635962));
#20228=CARTESIAN_POINT('Ctrl Pts',(98.6851918584676,1.27787389101413,-1.7957516002806));
#20229=CARTESIAN_POINT('Ctrl Pts',(98.6847418784087,1.27107283762284,-1.80057194470799));
#20230=CARTESIAN_POINT('Ctrl Pts',(98.6839033563689,1.25842339944557,-1.80943003554));
#20231=CARTESIAN_POINT('Ctrl Pts',(98.6835155255657,1.2525826443354,-1.81347821060342));
#20232=CARTESIAN_POINT('Ctrl Pts',(98.6826138300427,1.23902470306247,-1.82277835234845));
#20233=CARTESIAN_POINT('Ctrl Pts',(98.6820986217684,1.23129364758351,-1.82800959612674));
#20234=CARTESIAN_POINT('Ctrl Pts',(98.6804403429749,1.20645052773899,-1.84459067694046));
#20235=CARTESIAN_POINT('Ctrl Pts',(98.6792857088648,1.18921346119645,-1.85575023190175));
#20236=CARTESIAN_POINT('Ctrl Pts',(98.6728522086044,1.0933365106662,-1.91593819433007));
#20237=CARTESIAN_POINT('Ctrl Pts',(98.6673455919456,1.01182606062339,-1.96020639111566));
#20238=CARTESIAN_POINT('Ctrl Pts',(98.6517564085217,0.775927256615732,-2.06968069392965));
#20239=CARTESIAN_POINT('Ctrl Pts',(98.6416605152143,0.616515859598225,-2.12263144981644));
#20240=CARTESIAN_POINT('Ctrl Pts',(98.629725095709,0.41112898613636,-2.16573023022504));
#20241=CARTESIAN_POINT('Ctrl Pts',(98.6273486368494,0.369379979564882,-2.17324026584815));
#20242=CARTESIAN_POINT('Ctrl Pts',(98.6240108274908,0.309520200969144,-2.18223315509295));
#20243=CARTESIAN_POINT('Ctrl Pts',(98.6230186967612,0.291569405075992,-2.18470400917741));
#20244=CARTESIAN_POINT('Ctrl Pts',(98.6213367556113,0.260873037841006,-2.18854415190712));
#20245=CARTESIAN_POINT('Ctrl Pts',(98.6206434892773,0.248142467769818,-2.19002410309161));
#20246=CARTESIAN_POINT('Ctrl Pts',(98.619236957212,0.222158312181555,-2.19281532215628));
#20247=CARTESIAN_POINT('Ctrl Pts',(98.6185239993739,0.208904290057733,-2.19411767256596));
#20248=CARTESIAN_POINT('Ctrl Pts',(98.6167488067306,0.175701857908739,-2.19707658185456));
#20249=CARTESIAN_POINT('Ctrl Pts',(98.6156913515618,0.15574094826306,-2.19858168863068));
#20250=CARTESIAN_POINT('Ctrl Pts',(98.6114810564352,0.0755772956097627,
-2.20352899899307));
#20251=CARTESIAN_POINT('Ctrl Pts',(98.6083966205884,0.0152628608045295,
-2.20477205961372));
#20252=CARTESIAN_POINT('Ctrl Pts',(98.6000963612398,-0.150073761844254,
-2.201393329608));
#20253=CARTESIAN_POINT('Ctrl Pts',(98.595014195561,-0.254833118708533,-2.19173820956238));
#20254=CARTESIAN_POINT('Ctrl Pts',(98.5834992921154,-0.489914183120483,
-2.15298336325006));
#20255=CARTESIAN_POINT('Ctrl Pts',(98.5770940579482,-0.619073572472979,
-2.11945590433883));
#20256=CARTESIAN_POINT('Ctrl Pts',(98.5690944463103,-0.763459170958991,
-2.06764505706151));
#20257=CARTESIAN_POINT('Ctrl Pts',(98.5680262147203,-0.782421649149607,
-2.0605441740682));
#20258=CARTESIAN_POINT('Ctrl Pts',(98.5664523187556,-0.809838650084238,
-2.0498443136061));
#20259=CARTESIAN_POINT('Ctrl Pts',(98.5659581996391,-0.81837326267101,-2.04645194081454));
#20260=CARTESIAN_POINT('Ctrl Pts',(98.5650760520444,-0.833474404425227,
-2.04033990570651));
#20261=CARTESIAN_POINT('Ctrl Pts',(98.5646892974171,-0.84004932778919,-2.037641685651));
#20262=CARTESIAN_POINT('Ctrl Pts',(98.5638448545568,-0.854304212247811,
-2.03171103707455));
#20263=CARTESIAN_POINT('Ctrl Pts',(98.563386498473,-0.861978816997602,-2.0284668938879));
#20264=CARTESIAN_POINT('Ctrl Pts',(98.5620725519888,-0.883807706488205,
-2.01909332415812));
#20265=CARTESIAN_POINT('Ctrl Pts',(98.5612109887713,-0.897916020027165,
-2.01285883939544));
#20266=CARTESIAN_POINT('Ctrl Pts',(98.5535751592214,-1.02129427777264,-1.95678258886938));
#20267=CARTESIAN_POINT('Ctrl Pts',(98.546379264091,-1.12637686932969,-1.89823868162809));
#20268=CARTESIAN_POINT('Ctrl Pts',(98.5290866121702,-1.36558190948279,-1.73808934537798));
#20269=CARTESIAN_POINT('Ctrl Pts',(98.5190655536559,-1.49391390694665,-1.62911233654001));
#20270=CARTESIAN_POINT('Ctrl Pts',(98.5081331374325,-1.62715108873485,-1.48685178877377));
#20271=CARTESIAN_POINT('Ctrl Pts',(98.5066297714836,-1.64529206559808,-1.46675254156257));
#20272=CARTESIAN_POINT('Ctrl Pts',(98.5042484333055,-1.67372687560415,-1.43405670389279));
#20273=CARTESIAN_POINT('Ctrl Pts',(98.5033606414264,-1.68425917841203,-1.42167201703516));
#20274=CARTESIAN_POINT('Ctrl Pts',(98.5017898770111,-1.70276727077507,-1.39941439770102));
#20275=CARTESIAN_POINT('Ctrl Pts',(98.5011047377087,-1.71079654173152,-1.38958707432172));
#20276=CARTESIAN_POINT('Ctrl Pts',(98.4996748593877,-1.72745873617371,-1.3688302568602));
#20277=CARTESIAN_POINT('Ctrl Pts',(98.4989308516205,-1.73607386028385,-1.35788715330779));
#20278=CARTESIAN_POINT('Ctrl Pts',(98.496975007594,-1.75857008982103,-1.32874790009838));
#20279=CARTESIAN_POINT('Ctrl Pts',(98.4957702050007,-1.77227268978393,-1.31041570037055));
#20280=CARTESIAN_POINT('Ctrl Pts',(98.48966729184,-1.84082204429818,-1.21566355332151));
#20281=CARTESIAN_POINT('Ctrl Pts',(98.4849479027376,-1.89102417542894,-1.13599903080722));
#20282=CARTESIAN_POINT('Ctrl Pts',(98.4758414440255,-1.9796466965911,-0.97311889189785));
#20283=CARTESIAN_POINT('Ctrl Pts',(98.4714567605868,-2.01827668827651,-0.89023644646018));
#20284=CARTESIAN_POINT('Ctrl Pts',(98.4654624706985,-2.06347430166398,-0.775072277845698));
#20285=CARTESIAN_POINT('Ctrl Pts',(98.4638895505575,-2.07463180192088,-0.744691922107024));
#20286=CARTESIAN_POINT('Ctrl Pts',(98.458229562875,-2.11205466567206,-0.635416623754059));
#20287=CARTESIAN_POINT('Ctrl Pts',(98.4540767898702,-2.13451790430606,-0.555301615725078));
#20288=CARTESIAN_POINT('Ctrl Pts',(98.4489142210089,-2.15560438419302,-0.459573230050325));
#20289=CARTESIAN_POINT('Ctrl Pts',(98.4481226971001,-2.1586606226162,-0.444996749781833));
#20290=CARTESIAN_POINT('Ctrl Pts',(98.4468770938471,-2.16319133042813,-0.422241996652536));
#20291=CARTESIAN_POINT('Ctrl Pts',(98.4464285419477,-2.1647677248158,-0.414084204940365));
#20292=CARTESIAN_POINT('Ctrl Pts',(98.4455948862398,-2.16759507497236,-0.398995232940917));
#20293=CARTESIAN_POINT('Ctrl Pts',(98.4452105112397,-2.16885897862143,-0.392066743442667));
#20294=CARTESIAN_POINT('Ctrl Pts',(98.4443122653992,-2.17172094330413,-0.375940546699376));
#20295=CARTESIAN_POINT('Ctrl Pts',(98.4437970155783,-2.17329379221109,-0.366738648761557));
#20296=CARTESIAN_POINT('Ctrl Pts',(98.4421384610594,-2.17813973675719,-0.337261173484782));
#20297=CARTESIAN_POINT('Ctrl Pts',(98.4409835875036,-2.18118781046561,-0.316950288812622));
#20298=CARTESIAN_POINT('Ctrl Pts',(98.4345474382195,-2.19642817198285,-0.204731309135863));
#20299=CARTESIAN_POINT('Ctrl Pts',(98.4290382202955,-2.2030946212742,-0.112173498256287));
#20300=CARTESIAN_POINT('Ctrl Pts',(98.4134394400837,-2.20539454711444,0.148037288622614));
#20301=CARTESIAN_POINT('Ctrl Pts',(98.4033368297977,-2.18777093699505,0.315203614232164));
#20302=CARTESIAN_POINT('Ctrl Pts',(98.3914031458814,-2.14218503464559,0.520045485017039));
#20303=CARTESIAN_POINT('Ctrl Pts',(98.3890337785581,-2.13181320348286,0.561049766660444));
#20304=CARTESIAN_POINT('Ctrl Pts',(98.3857038047588,-2.11532527181567,0.619146736375997));
#20305=CARTESIAN_POINT('Ctrl Pts',(98.3847126229588,-2.11016860540951,0.636499938029204));
#20306=CARTESIAN_POINT('Ctrl Pts',(98.3830317990227,-2.10099787342105,0.666024101175495));
#20307=CARTESIAN_POINT('Ctrl Pts',(98.3823387122056,-2.09709044444314,0.678226986338901));
#20308=CARTESIAN_POINT('Ctrl Pts',(98.3809321338001,-2.08890376767203,0.703046598009524));
#20309=CARTESIAN_POINT('Ctrl Pts',(98.380218954289,-2.08461609096221,0.715659998599143));
#20310=CARTESIAN_POINT('Ctrl Pts',(98.3784424177545,-2.07359348359208,0.747146288312893));
#20311=CARTESIAN_POINT('Ctrl Pts',(98.3773838561946,-2.0667149745291,0.765967858754301));
#20312=CARTESIAN_POINT('Ctrl Pts',(98.3731625853744,-2.03804429409815,0.841219637864688));
#20313=CARTESIAN_POINT('Ctrl Pts',(98.3700687526667,-2.01418906691081,0.896837915314152));
#20314=CARTESIAN_POINT('Ctrl Pts',(98.3617318569797,-1.94247682190186,1.04668878335903));
#20315=CARTESIAN_POINT('Ctrl Pts',(98.3566240826993,-1.89008695378227,1.13857212896967));
#20316=CARTESIAN_POINT('Ctrl Pts',(98.3451202830752,-1.75764496482616,1.33634837653496));
#20317=CARTESIAN_POINT('Ctrl Pts',(98.3387500363932,-1.67422775834202,1.43947785070547));
#20318=CARTESIAN_POINT('Ctrl Pts',(98.3307919507877,-1.5679816205828,1.54901885236369));
#20319=CARTESIAN_POINT('Ctrl Pts',(98.3297239989432,-1.55368903399983,1.56335411720036));
#20320=CARTESIAN_POINT('Ctrl Pts',(98.3281504435174,-1.53262879165441,1.58390319062292));
#20321=CARTESIAN_POINT('Ctrl Pts',(98.3276563783816,-1.5260161474922,1.59027514656847));
#20322=CARTESIAN_POINT('Ctrl Pts',(98.3267742919527,-1.514215480365,1.6015049143617));
#20323=CARTESIAN_POINT('Ctrl Pts',(98.3263875438814,-1.50904351327845,1.60637921590838));
#20324=CARTESIAN_POINT('Ctrl Pts',(98.3255430713505,-1.49775622519392,1.61691426052723));
#20325=CARTESIAN_POINT('Ctrl Pts',(98.3250846785528,-1.49163244001975,1.62256528226141));
#20326=CARTESIAN_POINT('Ctrl Pts',(98.3237705218262,-1.4740799326161,1.63857937287407));
#20327=CARTESIAN_POINT('Ctrl Pts',(98.3229087821879,-1.46257446558192,1.64885715397298));
#20328=CARTESIAN_POINT('Ctrl Pts',(98.3194014515235,-1.4157177157993,1.68983777408038));
#20329=CARTESIAN_POINT('Ctrl Pts',(98.3166956872643,-1.3795019278426,1.71952964731155));
#20330=CARTESIAN_POINT('Ctrl Pts',(98.3071287479511,-1.25017169014619,1.81884588628619));
#20331=CARTESIAN_POINT('Ctrl Pts',(98.3000805206949,-1.15251785433927,1.88224104938039));
#20332=CARTESIAN_POINT('Ctrl Pts',(98.2851294875688,-0.932783051509522,
2.00135119430274));
#20333=CARTESIAN_POINT('Ctrl Pts',(98.2772965716504,-0.809676421049263,
2.05424547171919));
#20334=CARTESIAN_POINT('Ctrl Pts',(98.2684789473926,-0.659204908025221,
2.10325129947497));
#20335=CARTESIAN_POINT('Ctrl Pts',(98.2671253969096,-0.635766294878183,
2.11045455444487));
#20336=CARTESIAN_POINT('Ctrl Pts',(98.2649962753974,-0.598363214710584,
2.12126973240286));
#20337=CARTESIAN_POINT('Ctrl Pts',(98.2642124174512,-0.584475578760371,
2.12513814281748));
#20338=CARTESIAN_POINT('Ctrl Pts',(98.2627581545978,-0.558494925302232,
2.1321011235284));
#20339=CARTESIAN_POINT('Ctrl Pts',(98.2620866696422,-0.546411704121667,
2.13522973963945));
#20340=CARTESIAN_POINT('Ctrl Pts',(98.2605811568599,-0.519128057805538,
2.14204731434691));
#20341=CARTESIAN_POINT('Ctrl Pts',(98.2597490522509,-0.503913545915732,
2.14567746706132));
#20342=CARTESIAN_POINT('Ctrl Pts',(98.2580330262032,-0.472266649206409,
2.15287317236696));
#20343=CARTESIAN_POINT('Ctrl Pts',(98.257149951911,-0.455829488286515,2.15641326797312));
#20344=CARTESIAN_POINT('Ctrl Pts',(98.2539901320892,-0.396493389044315,
2.16848379443232));
#20345=CARTESIAN_POINT('Ctrl Pts',(98.2517470004201,-0.353382049824391,
2.17592518692529));
#20346=CARTESIAN_POINT('Ctrl Pts',(98.2442924541097,-0.207365264913901,
2.1966743374597));
#20347=CARTESIAN_POINT('Ctrl Pts',(98.2392465740022,-0.103749118601317,
2.20399999999769));
#20348=CARTESIAN_POINT('Ctrl Pts',(98.2342289786285,-4.90931427454822E-11,
2.204));
#20349=CARTESIAN_POINT('Ctrl Pts',(98.1265335566918,1.1079161893468E-10,
2.204));
#20350=CARTESIAN_POINT('Ctrl Pts',(98.1342675812916,-0.129411528099454,
2.20400000000651));
#20351=CARTESIAN_POINT('Ctrl Pts',(98.1418387474841,-0.258588760702719,
2.1926023181208));
#20352=CARTESIAN_POINT('Ctrl Pts',(98.150067141124,-0.403932858849224,2.16674517480458));
#20353=CARTESIAN_POINT('Ctrl Pts',(98.1510734060491,-0.421789255152345,
2.16334007015691));
#20354=CARTESIAN_POINT('Ctrl Pts',(98.15298752015,-0.455908821504527,2.15639515867179));
#20355=CARTESIAN_POINT('Ctrl Pts',(98.1538964368564,-0.472177959630861,
2.15289129538556));
#20356=CARTESIAN_POINT('Ctrl Pts',(98.1554946094833,-0.500898509638879,
2.14636455447198));
#20357=CARTESIAN_POINT('Ctrl Pts',(98.1561862344795,-0.513366032779234,
2.1434167685539));
#20358=CARTESIAN_POINT('Ctrl Pts',(98.1576317495377,-0.539500125647402,
2.1369965891951));
#20359=CARTESIAN_POINT('Ctrl Pts',(98.1583848697209,-0.553160533742675,
2.13350140482032));
#20360=CARTESIAN_POINT('Ctrl Pts',(98.1603699530106,-0.58927581628369,2.12389067266181));
#20361=CARTESIAN_POINT('Ctrl Pts',(98.1615946068978,-0.611669285116579,
2.117550074312));
#20362=CARTESIAN_POINT('Ctrl Pts',(98.1673981307745,-0.718237965388948,
2.08554403079052));
#20363=CARTESIAN_POINT('Ctrl Pts',(98.1718234480369,-0.800929964921452,
2.05520632162096));
#20364=CARTESIAN_POINT('Ctrl Pts',(98.183017280322,-1.0093104866917,1.96426246989302));
#20365=CARTESIAN_POINT('Ctrl Pts',(98.1896086042554,-1.13144832429597,1.89653827803078));
#20366=CARTESIAN_POINT('Ctrl Pts',(98.2000944872558,-1.30696649579322,1.77619046466001));
#20367=CARTESIAN_POINT('Ctrl Pts',(98.2037891419838,-1.36544079150786,1.73164185762113));
#20368=CARTESIAN_POINT('Ctrl Pts',(98.2084392819634,-1.4328695058533,1.67472964239195));
#20369=CARTESIAN_POINT('Ctrl Pts',(98.2092251628545,-1.44406632968273,1.66508462483534));
#20370=CARTESIAN_POINT('Ctrl Pts',(98.2104618405022,-1.461357408337,1.64988439104084));
#20371=CARTESIAN_POINT('Ctrl Pts',(98.2109071797518,-1.46751910980342,1.64440616532635));
#20372=CARTESIAN_POINT('Ctrl Pts',(98.2117469678895,-1.47901285064892,1.63407129713722));
#20373=CARTESIAN_POINT('Ctrl Pts',(98.2121408210175,-1.48435195829846,1.62922290529164));
#20374=CARTESIAN_POINT('Ctrl Pts',(98.213061270069,-1.49671229760999,1.61788741195389));
#20375=CARTESIAN_POINT('Ctrl Pts',(98.2135893117975,-1.50371523724513,1.61138073028224));
#20376=CARTESIAN_POINT('Ctrl Pts',(98.2153467468011,-1.52674259607246,1.58970435823022));
#20377=CARTESIAN_POINT('Ctrl Pts',(98.2165897252916,-1.54258104587969,1.57434003389174));
#20378=CARTESIAN_POINT('Ctrl Pts',(98.2296109696313,-1.70425064945158,1.41272805708928));
#20379=CARTESIAN_POINT('Ctrl Pts',(98.2424133887902,-1.82906894496877,1.24691060655508));
#20380=CARTESIAN_POINT('Ctrl Pts',(98.2594922207184,-1.96994946183549,0.992011775991571));
#20381=CARTESIAN_POINT('Ctrl Pts',(98.2643457288979,-2.0066128547686,0.915584904883031));
#20382=CARTESIAN_POINT('Ctrl Pts',(98.270292549029,-2.04729595690345,0.816514988206113));
#20383=CARTESIAN_POINT('Ctrl Pts',(98.2715254177405,-2.05548648621096,0.795671300483503));
#20384=CARTESIAN_POINT('Ctrl Pts',(98.2735068928136,-2.06824798181319,0.761682224342442));
#20385=CARTESIAN_POINT('Ctrl Pts',(98.2742619909356,-2.07301447571637,0.748612397101283));
#20386=CARTESIAN_POINT('Ctrl Pts',(98.2757075522665,-2.08195077234184,0.723368879750863));
#20387=CARTESIAN_POINT('Ctrl Pts',(98.2763985819378,-2.08613832529582,0.711202117616855));
#20388=CARTESIAN_POINT('Ctrl Pts',(98.2779815135341,-2.09553368901123,0.68310713666743));
#20389=CARTESIAN_POINT('Ctrl Pts',(98.2788709297653,-2.10066690212705,0.667154696577519));
#20390=CARTESIAN_POINT('Ctrl Pts',(98.2817427909987,-2.11675758819062,0.615121989960742));
#20391=CARTESIAN_POINT('Ctrl Pts',(98.2837011133369,-2.12697152891783,0.578817832961619));
#20392=CARTESIAN_POINT('Ctrl Pts',(98.2945026204928,-2.1788408379171,0.374480164961383));
#20393=CARTESIAN_POINT('Ctrl Pts',(98.3027196356053,-2.20151638021777,0.202264551132464));
#20394=CARTESIAN_POINT('Ctrl Pts',(98.3157245974498,-2.20505702532042,-0.0652950997036932));
#20395=CARTESIAN_POINT('Ctrl Pts',(98.3203750544143,-2.20023264076704,-0.159727814560823));
#20396=CARTESIAN_POINT('Ctrl Pts',(98.3263790455512,-2.18697490316926,-0.274206470406807));
#20397=CARTESIAN_POINT('Ctrl Pts',(98.3274753043682,-2.18429054031064,-0.29482738880053));
#20398=CARTESIAN_POINT('Ctrl Pts',(98.3290913257518,-2.17996439454056,-0.324746514266223));
#20399=CARTESIAN_POINT('Ctrl Pts',(98.3295989385246,-2.17855392680965,-0.334077597861353));
#20400=CARTESIAN_POINT('Ctrl Pts',(98.3304986672856,-2.1759649227379,-0.350491377905123));
#20401=CARTESIAN_POINT('Ctrl Pts',(98.3308893715168,-2.1748116417929,-0.357577784837447));
#20402=CARTESIAN_POINT('Ctrl Pts',(98.3317428795821,-2.1722298504236,-0.372967090180427));
#20403=CARTESIAN_POINT('Ctrl Pts',(98.3322063691222,-2.17078837638064,-0.381267351817282));
#20404=CARTESIAN_POINT('Ctrl Pts',(98.3335126844337,-2.16661449004253,-0.40451006723062));
#20405=CARTESIAN_POINT('Ctrl Pts',(98.3343611677306,-2.16377518387219,-0.41943255773293));
#20406=CARTESIAN_POINT('Ctrl Pts',(98.3403770994855,-2.14273173726806,-0.524124657208725));
#20407=CARTESIAN_POINT('Ctrl Pts',(98.3457914881777,-2.11910256302468,-0.6127047896272));
#20408=CARTESIAN_POINT('Ctrl Pts',(98.3525790651776,-2.08309050824252,-0.720297624474304));
#20409=CARTESIAN_POINT('Ctrl Pts',(98.3538915189407,-2.07583726940177,-0.740941530666156));
#20410=CARTESIAN_POINT('Ctrl Pts',(98.3604467504533,-2.03811916092529,-0.84338960349826));
#20411=CARTESIAN_POINT('Ctrl Pts',(98.3656997813867,-2.00311934991906,-0.923444474573782));
#20412=CARTESIAN_POINT('Ctrl Pts',(98.3766987344221,-1.91854314998671,-1.08930524957409));
#20413=CARTESIAN_POINT('Ctrl Pts',(98.382403215317,-1.86774241272555,-1.17428110053408));
#20414=CARTESIAN_POINT('Ctrl Pts',(98.389198556046,-1.79811950705285,-1.27472572596009));
#20415=CARTESIAN_POINT('Ctrl Pts',(98.3904833038852,-1.78453587655683,-1.29367353004006));
#20416=CARTESIAN_POINT('Ctrl Pts',(98.3925270563952,-1.76225270172871,-1.32373730972213));
#20417=CARTESIAN_POINT('Ctrl Pts',(98.3932933207587,-1.75374282170363,-1.33499107796208));
#20418=CARTESIAN_POINT('Ctrl Pts',(98.3947471583142,-1.73730202930718,-1.35630443517149));
#20419=CARTESIAN_POINT('Ctrl Pts',(98.3954354474019,-1.72939036060438,-1.36637807804118));
#20420=CARTESIAN_POINT('Ctrl Pts',(98.3969943124829,-1.7111819669325,-1.38915065226837));
#20421=CARTESIAN_POINT('Ctrl Pts',(98.3978626591386,-1.70083080304664,-1.40180521382827));
#20422=CARTESIAN_POINT('Ctrl Pts',(98.400155687419,-1.67294973430274,-1.43512701230067));
#20423=CARTESIAN_POINT('Ctrl Pts',(98.4015704982026,-1.6551775752626,-1.45558841459629));
#20424=CARTESIAN_POINT('Ctrl Pts',(98.4116766108309,-1.52425221736762,-1.60082557113283));
#20425=CARTESIAN_POINT('Ctrl Pts',(98.4197437546766,-1.39750499458331,-1.7125921598198));
#20426=CARTESIAN_POINT('Ctrl Pts',(98.4336719667384,-1.16138494391914,-1.87697146363944));
#20427=CARTESIAN_POINT('Ctrl Pts',(98.4394849649576,-1.05815698673902,-1.93704262093118));
#20428=CARTESIAN_POINT('Ctrl Pts',(98.4465749215195,-0.936589367455986,
-1.99515845338046));
#20429=CARTESIAN_POINT('Ctrl Pts',(98.4473992943453,-0.922516402084734,
-2.00170436333038));
#20430=CARTESIAN_POINT('Ctrl Pts',(98.4486834078557,-0.900719733283858,
-2.01156421051943));
#20431=CARTESIAN_POINT('Ctrl Pts',(98.4491369934123,-0.893043975208039,
-2.01498363878429));
#20432=CARTESIAN_POINT('Ctrl Pts',(98.4499833236967,-0.878770921557868,
-2.02124448400393));
#20433=CARTESIAN_POINT('Ctrl Pts',(98.4503753567422,-0.872179073368367,
-2.02409763991019));
#20434=CARTESIAN_POINT('Ctrl Pts',(98.451280009738,-0.857011455726024,-2.0305748054557));
#20435=CARTESIAN_POINT('Ctrl Pts',(98.4517939143316,-0.848426563812317,
-2.03417674630099));
#20436=CARTESIAN_POINT('Ctrl Pts',(98.4534571093831,-0.820732479924208,
-2.04559047256281));
#20437=CARTESIAN_POINT('Ctrl Pts',(98.4546181289027,-0.801536799408227,
-2.05318798005866));
#20438=CARTESIAN_POINT('Ctrl Pts',(98.4627764661831,-0.667354874914458,
-2.10412778066878));
#20439=CARTESIAN_POINT('Ctrl Pts',(98.470173957133,-0.549034050412121,-2.13805365291387));
#20440=CARTESIAN_POINT('Ctrl Pts',(98.4842669946737,-0.318918408600111,
-2.18366435939356));
#20441=CARTESIAN_POINT('Ctrl Pts',(98.4909452494111,-0.207821346029025,
-2.19702372319374));
#20442=CARTESIAN_POINT('Ctrl Pts',(98.4998252001992,-0.0543381810846674,
-2.20372813043171));
#20443=CARTESIAN_POINT('Ctrl Pts',(98.5022150687436,-0.0124482554290852,
-2.20436287184061));
#20444=CARTESIAN_POINT('Ctrl Pts',(98.5063633339066,0.0613422884274224,
-2.20337724793752));
#20445=CARTESIAN_POINT('Ctrl Pts',(98.5081360938787,0.0932363403105149,
-2.20225822926894));
#20446=CARTESIAN_POINT('Ctrl Pts',(98.5107587395572,0.140948626565379,-2.19954577131933));
#20447=CARTESIAN_POINT('Ctrl Pts',(98.5116247370679,0.156791253346352,-2.19847325135941));
#20448=CARTESIAN_POINT('Ctrl Pts',(98.5131690767354,0.185196754578092,-2.19624162664492));
#20449=CARTESIAN_POINT('Ctrl Pts',(98.5138493683941,0.197763766157444,-2.19514569505861));
#20450=CARTESIAN_POINT('Ctrl Pts',(98.5153049155017,0.224764591735997,-2.19255727789587));
#20451=CARTESIAN_POINT('Ctrl Pts',(98.5160790447494,0.239194523060699,-2.19103001632704));
#20452=CARTESIAN_POINT('Ctrl Pts',(98.5181506815756,0.277987802607225,-2.18653632580843));
#20453=CARTESIAN_POINT('Ctrl Pts',(98.5194398493154,0.302318776571269,-2.18330523365501));
#20454=CARTESIAN_POINT('Ctrl Pts',(98.5274372040842,0.454300813346942,-2.16053295161724));
#20455=CARTESIAN_POINT('Ctrl Pts',(98.533790594079,0.580086093700449,-2.13021052558156));
#20456=CARTESIAN_POINT('Ctrl Pts',(98.5446281566084,0.7919950490614,-2.05894978114176));
#20457=CARTESIAN_POINT('Ctrl Pts',(98.5491501803657,0.879457511349592,-2.02313714585559));
#20458=CARTESIAN_POINT('Ctrl Pts',(98.5562919479058,1.00985654916164,-1.95968537288833));
#20459=CARTESIAN_POINT('Ctrl Pts',(98.5588195989674,1.05458323501026,-1.93598312938727));
#20460=CARTESIAN_POINT('Ctrl Pts',(98.5624990818,1.11676209727599,-1.9002380042372));
#20461=CARTESIAN_POINT('Ctrl Pts',(98.563594325884,1.13491932265903,-1.88944968940844));
#20462=CARTESIAN_POINT('Ctrl Pts',(98.565559642031,1.16680275306233,-1.86988040901389));
#20463=CARTESIAN_POINT('Ctrl Pts',(98.5664238960406,1.18059206995939,-1.86120491668689));
#20464=CARTESIAN_POINT('Ctrl Pts',(98.5677570591446,1.20148133404075,-1.84773698012256));
#20465=CARTESIAN_POINT('Ctrl Pts',(98.568219051284,1.20865189770259,-1.84305451057076));
#20466=CARTESIAN_POINT('Ctrl Pts',(98.5690726596788,1.22177046123197,-1.83437844136985));
#20467=CARTESIAN_POINT('Ctrl Pts',(98.569463449992,1.22772649176283,-1.8303974932565));
#20468=CARTESIAN_POINT('Ctrl Pts',(98.5703629520683,1.24132292718394,-1.82121356104591));
#20469=CARTESIAN_POINT('Ctrl Pts',(98.5708729105653,1.2489500661958,-1.81599151163634));
#20470=CARTESIAN_POINT('Ctrl Pts',(98.5724813864516,1.2727629960148,-1.79946661263661));
#20471=CARTESIAN_POINT('Ctrl Pts',(98.5735904569145,1.28882948430159,-1.78799447401757));
#20472=CARTESIAN_POINT('Ctrl Pts',(98.5826342482094,1.41723715804116,-1.69367610750241));
#20473=CARTESIAN_POINT('Ctrl Pts',(98.5910899860241,1.52162320203072,-1.60054921876053));
#20474=CARTESIAN_POINT('Ctrl Pts',(98.6084357380205,1.71814274201587,-1.38851083312785));
#20475=CARTESIAN_POINT('Ctrl Pts',(98.6172575115556,1.80837930788489,-1.26876086808271));
#20476=CARTESIAN_POINT('Ctrl Pts',(98.6270056699343,1.89887843463933,-1.11915821190153));
#20477=CARTESIAN_POINT('Ctrl Pts',(98.6284010166433,1.91158402809286,-1.0973153563946));
#20478=CARTESIAN_POINT('Ctrl Pts',(98.630577250089,1.93099870624075,-1.06257753712468));
#20479=CARTESIAN_POINT('Ctrl Pts',(98.6313671430813,1.9379603876628,-1.04982692667709));
#20480=CARTESIAN_POINT('Ctrl Pts',(98.6328409811135,1.95078688807377,-1.02577222605599));
#20481=CARTESIAN_POINT('Ctrl Pts',(98.6335259377552,1.95668075776525,-1.01448438335463));
#20482=CARTESIAN_POINT('Ctrl Pts',(98.6350592026763,1.96971977815122,-0.988975859477251));
#20483=CARTESIAN_POINT('Ctrl Pts',(98.6359055381135,1.97680943560853,-0.974727514930891));
#20484=CARTESIAN_POINT('Ctrl Pts',(98.6383874232418,1.99727270343902,-0.932459972355329));
#20485=CARTESIAN_POINT('Ctrl Pts',(98.6400079185816,2.01020960063278,-0.904233011257104));
#20486=CARTESIAN_POINT('Ctrl Pts',(98.6489161915457,2.07880822623853,-0.745802763263234));
#20487=CARTESIAN_POINT('Ctrl Pts',(98.6557890423879,2.12241915957824,-0.61074300159894));
#20488=CARTESIAN_POINT('Ctrl Pts',(98.6675187849966,2.17443774992763,-0.373700150524359));
#20489=CARTESIAN_POINT('Ctrl Pts',(98.6723843592178,2.18928440543749,-0.273610662932377));
#20490=CARTESIAN_POINT('Ctrl Pts',(98.6790845909202,2.19972608287166,-0.140889251224202));
#20491=CARTESIAN_POINT('Ctrl Pts',(98.6807205305533,2.20154323439667,-0.108866139005686));
#20492=CARTESIAN_POINT('Ctrl Pts',(98.6835495221358,2.20344080942994,-0.0544542376564715));
#20493=CARTESIAN_POINT('Ctrl Pts',(98.6847268049499,2.20388005529775,-0.032082558129561));
#20494=CARTESIAN_POINT('Ctrl Pts',(98.6864405806421,2.20402141575721,6.99580985433863E-6));
#20495=CARTESIAN_POINT('Ctrl Pts',(98.6869627701434,2.20399996797403,0.00972292075741761));
#20496=CARTESIAN_POINT('Ctrl Pts',(98.6878786850192,2.20385068625488,0.0266485667196372));
#20497=CARTESIAN_POINT('Ctrl Pts',(98.688270815811,2.20375171214969,0.0338582872283345));
#20498=CARTESIAN_POINT('Ctrl Pts',(98.6891160501953,2.20346360134124,0.049317817146144));
#20499=CARTESIAN_POINT('Ctrl Pts',(98.6895697138049,2.20326351817185,0.0575669562826086));
#20500=CARTESIAN_POINT('Ctrl Pts',(98.6908228789141,2.20258652479216,0.0802279942411993));
#20501=CARTESIAN_POINT('Ctrl Pts',(98.6916273564445,2.20201450063624,0.0946363922203018));
#20502=CARTESIAN_POINT('Ctrl Pts',(98.6962328716195,2.19796389806364,0.176411710906731));
#20503=CARTESIAN_POINT('Ctrl Pts',(98.7001685095041,2.19153553469335,0.243591567500691));
#20504=CARTESIAN_POINT('Ctrl Pts',(98.7120803409204,2.16324177352094,0.442512598869018));
#20505=CARTESIAN_POINT('Ctrl Pts',(98.7201986022711,2.13247999570725,0.572681161522842));
#20506=CARTESIAN_POINT('Ctrl Pts',(98.7320161394143,2.0690473074637,0.762282136242877));
#20507=CARTESIAN_POINT('Ctrl Pts',(98.735885247166,2.04512656337665,0.824311401617631));
#20508=CARTESIAN_POINT('Ctrl Pts',(98.7422221416428,2.00044362563261,0.926201235584311));
#20509=CARTESIAN_POINT('Ctrl Pts',(98.7447347374067,1.98120151032895,0.966676996040508));
#20510=CARTESIAN_POINT('Ctrl Pts',(98.7482026347796,1.95247538404131,1.02263541791487));
#20511=CARTESIAN_POINT('Ctrl Pts',(98.7491931368884,1.94401491551415,1.03862859535656));
#20512=CARTESIAN_POINT('Ctrl Pts',(98.7508854067987,1.92912050406717,1.06596437707166));
#20513=CARTESIAN_POINT('Ctrl Pts',(98.7515904868767,1.92278116495564,1.0773572175992));
#20514=CARTESIAN_POINT('Ctrl Pts',(98.7530205606184,1.90965181112561,1.10046778410405));
#20515=CARTESIAN_POINT('Ctrl Pts',(98.7537452384513,1.90285413595174,1.11218053037046));
#20516=CARTESIAN_POINT('Ctrl Pts',(98.755565429487,1.88541736165545,1.14159710582605));
#20517=CARTESIAN_POINT('Ctrl Pts',(98.7566557402799,1.87463643993571,1.15921561248863));
#20518=CARTESIAN_POINT('Ctrl Pts',(98.7608459184468,1.83191954736191,1.22687000297117));
#20519=CARTESIAN_POINT('Ctrl Pts',(98.7638805107272,1.79821388078437,1.27576128015598));
#20520=CARTESIAN_POINT('Ctrl Pts',(98.7744506251936,1.67175074234055,1.44421250114368));
#20521=CARTESIAN_POINT('Ctrl Pts',(98.7816221031447,1.56871747569274,1.55551476246047));
#20522=CARTESIAN_POINT('Ctrl Pts',(98.7936205643539,1.38385176687156,1.71801273736785));
#20523=CARTESIAN_POINT('Ctrl Pts',(98.7983214930345,1.30864610294954,1.7759659805567));
#20524=CARTESIAN_POINT('Ctrl Pts',(98.8041125989796,1.21739220972108,1.83733537185422));
#20525=CARTESIAN_POINT('Ctrl Pts',(98.8049169659176,1.20474699581101,1.84565156838166));
#20526=CARTESIAN_POINT('Ctrl Pts',(98.8061764357197,1.18501835980409,1.85833708695035));
#20527=CARTESIAN_POINT('Ctrl Pts',(98.8066257506477,1.17799391539236,1.86279778089008));
#20528=CARTESIAN_POINT('Ctrl Pts',(98.8074686121048,1.16484744764102,1.87104201365884));
#20529=CARTESIAN_POINT('Ctrl Pts',(98.8078615064587,1.15873195854906,1.87483546913788));
#20530=CARTESIAN_POINT('Ctrl Pts',(98.8087739847425,1.14455672275558,1.88353256211609));
#20531=CARTESIAN_POINT('Ctrl Pts',(98.8092949337136,1.13648395243948,1.88841447339648));
#20532=CARTESIAN_POINT('Ctrl Pts',(98.81096009368,1.11073387245209,1.90376161125347));
#20533=CARTESIAN_POINT('Ctrl Pts',(98.8121157764305,1.09294195659972,1.91403130216732));
#20534=CARTESIAN_POINT('Ctrl Pts',(98.8197015382937,0.976467970602844,1.97910790887207));
#20535=CARTESIAN_POINT('Ctrl Pts',(98.8264692785218,0.873849565938286,2.02650950660868));
#20536=CARTESIAN_POINT('Ctrl Pts',(98.8401539050951,0.660335626333366,2.10589222575151));
#20537=CARTESIAN_POINT('Ctrl Pts',(98.8470479344221,0.549632627971197,2.13745950361733));
#20538=CARTESIAN_POINT('Ctrl Pts',(98.8563490584958,0.392518121763679,2.16923995105505));
#20539=CARTESIAN_POINT('Ctrl Pts',(98.8589450720198,0.347801460762961,2.17685713454391));
#20540=CARTESIAN_POINT('Ctrl Pts',(98.8634093806414,0.269309786197768,2.18774697928226));
#20541=CARTESIAN_POINT('Ctrl Pts',(98.8652952713311,0.235636061696432,2.19162962945356));
#20542=CARTESIAN_POINT('Ctrl Pts',(98.8680497044701,0.185699217557624,2.19622311945774));
#20543=CARTESIAN_POINT('Ctrl Pts',(98.8689368360128,0.169497363816221,2.1975329015674));
#20544=CARTESIAN_POINT('Ctrl Pts',(98.8705106482872,0.140547595467022,2.19955116591884));
#20545=CARTESIAN_POINT('Ctrl Pts',(98.8711994524446,0.127805347448724,2.20032833023113));
#20546=CARTESIAN_POINT('Ctrl Pts',(98.8726530943252,0.100765636899738,2.20174182956284));
#20547=CARTESIAN_POINT('Ctrl Pts',(98.8734170096334,0.0864672385194966,
2.20234970599652));
#20548=CARTESIAN_POINT('Ctrl Pts',(98.8754536893319,0.0481177909160257,
2.20360602294779));
#20549=CARTESIAN_POINT('Ctrl Pts',(98.8767184847374,0.0240600261670358,
2.204));
#20550=CARTESIAN_POINT('Ctrl Pts',(98.8779717715633,2.72446158072696E-13,
2.204));
#20551=CARTESIAN_POINT('Origin',(66.9212607628943,0.,0.));
#20552=CARTESIAN_POINT('',(99.7342548474101,-0.00178926204916046,2.20399927371615));
#20553=CARTESIAN_POINT('',(99.6260484068026,-0.00167252030352779,2.20399936539824));
#20554=CARTESIAN_POINT('',(66.9212607628943,-2.69912154532077E-16,2.204));
#20555=CARTESIAN_POINT('Ctrl Pts',(99.7351509568116,-0.00173560988551529,
2.2039993166193));
#20556=CARTESIAN_POINT('Ctrl Pts',(99.7325859424291,0.0411057575387971,
2.20403305342686));
#20557=CARTESIAN_POINT('Ctrl Pts',(99.7300092536942,0.0839392511825805,
2.20281765734755));
#20558=CARTESIAN_POINT('Ctrl Pts',(99.7179214914535,0.284885301152986,2.19124591586051));
#20559=CARTESIAN_POINT('Ctrl Pts',(99.7085400364541,0.44164106551191,2.16510665179586));
#20560=CARTESIAN_POINT('Ctrl Pts',(99.6982903113705,0.618661119182372,2.11554169667784));
#20561=CARTESIAN_POINT('Ctrl Pts',(99.6968906911373,0.642946224384297,2.10828804457973));
#20562=CARTESIAN_POINT('Ctrl Pts',(99.6947133307707,0.680892380503623,2.09623732762893));
#20563=CARTESIAN_POINT('Ctrl Pts',(99.6939264832767,0.694639956523387,2.09172194911354));
#20564=CARTESIAN_POINT('Ctrl Pts',(99.6924615589777,0.720295338562194,2.08301463219413));
#20565=CARTESIAN_POINT('Ctrl Pts',(99.6917824474597,0.732213468258517,2.07885516060639));
#20566=CARTESIAN_POINT('Ctrl Pts',(99.6902665539754,0.758867791840349,2.06929504226411));
#20567=CARTESIAN_POINT('Ctrl Pts',(99.6894316516828,0.773583436864061,2.06383889411998));
#20568=CARTESIAN_POINT('Ctrl Pts',(99.6869973639709,0.81657854801253,2.04737303495592));
#20569=CARTESIAN_POINT('Ctrl Pts',(99.6854122392978,0.844690948101202,2.03593570341873));
#20570=CARTESIAN_POINT('Ctrl Pts',(99.675702382682,1.01732104502677,1.96151088162598));
#20571=CARTESIAN_POINT('Ctrl Pts',(99.6681082105479,1.1549697772068,1.88375071690905));
#20572=CARTESIAN_POINT('Ctrl Pts',(99.6561640965481,1.35566529463431,1.74004067616937));
#20573=CARTESIAN_POINT('Ctrl Pts',(99.6518383342577,1.42495465145616,1.68376731047383));
#20574=CARTESIAN_POINT('Ctrl Pts',(99.6458244657953,1.51264713864155,1.60324896397048));
#20575=CARTESIAN_POINT('Ctrl Pts',(99.6442955464792,1.53424003292068,1.58259785971806));
#20576=CARTESIAN_POINT('Ctrl Pts',(99.6416563138614,1.57014997311557,1.54682841870791));
#20577=CARTESIAN_POINT('Ctrl Pts',(99.6405598584906,1.58468506746144,1.53193415998323));
#20578=CARTESIAN_POINT('Ctrl Pts',(99.6389614448569,1.60527763874894,1.5102260531971));
#20579=CARTESIAN_POINT('Ctrl Pts',(99.6384717809574,1.61150755697306,1.50357654183861));
#20580=CARTESIAN_POINT('Ctrl Pts',(99.6379747759479,1.61774924879298,1.49683111077629));
#20581=CARTESIAN_POINT('Ctrl Pts',(99.6379705318936,1.61780254224925,1.49677351007088));
#20582=CARTESIAN_POINT('Ctrl Pts',(99.6379620191038,1.6179094271203,1.49665797424254));
#20583=CARTESIAN_POINT('Ctrl Pts',(99.6379577503651,1.61796301850719,1.49660003907912));
#20584=CARTESIAN_POINT('Ctrl Pts',(99.6379491869644,1.61807051462472,1.49648381748856));
#20585=CARTESIAN_POINT('Ctrl Pts',(99.6379448922994,1.61812441931998,1.49642553102498));
#20586=CARTESIAN_POINT('Ctrl Pts',(99.637936275772,1.61823255782403,1.49630858955632));
#20587=CARTESIAN_POINT('Ctrl Pts',(99.6379319539071,1.61828679158838,1.4962499345204));
#20588=CARTESIAN_POINT('Ctrl Pts',(99.637539784944,1.62320743882082,1.49092756337933));
#20589=CARTESIAN_POINT('Ctrl Pts',(99.637150012691,1.62804807099266,1.48564022107006));
#20590=CARTESIAN_POINT('Ctrl Pts',(99.6363142056768,1.63831997983979,1.47430989186838));
#20591=CARTESIAN_POINT('Ctrl Pts',(99.6358676563816,1.64374368295239,1.46826043807011));
#20592=CARTESIAN_POINT('Ctrl Pts',(99.6346422525498,1.65845689987352,1.45166600940023));
#20593=CARTESIAN_POINT('Ctrl Pts',(99.6338587137178,1.66767904862106,1.44106212964295));
#20594=CARTESIAN_POINT('Ctrl Pts',(99.6295997589348,1.71685551986327,1.38341341505241));
#20595=CARTESIAN_POINT('Ctrl Pts',(99.6260115858911,1.7549188385564,1.33479743461425));
#20596=CARTESIAN_POINT('Ctrl Pts',(99.6145804532381,1.86766792043124,1.17761794910495));
#20597=CARTESIAN_POINT('Ctrl Pts',(99.6065678819278,1.93469709288563,1.06391543316853));
#20598=CARTESIAN_POINT('Ctrl Pts',(99.5936239071278,2.02828823111083,0.866693440372134));
#20599=CARTESIAN_POINT('Ctrl Pts',(99.5885840933124,2.06076594912135,0.786356740338615));
#20600=CARTESIAN_POINT('Ctrl Pts',(99.5816406607288,2.10005003095095,0.66987076894729));
#20601=CARTESIAN_POINT('Ctrl Pts',(99.5796144997086,2.11081131029522,0.635147867206938));
#20602=CARTESIAN_POINT('Ctrl Pts',(99.5767031442401,2.12523160905694,0.58419380240255));
#20603=CARTESIAN_POINT('Ctrl Pts',(99.5757960109156,2.12957319782394,0.568163539225504));
#20604=CARTESIAN_POINT('Ctrl Pts',(99.5742052488167,2.13691580318684,0.539785391838033));
#20605=CARTESIAN_POINT('Ctrl Pts',(99.5735192186002,2.1399919603836,0.527457901715318));
#20606=CARTESIAN_POINT('Ctrl Pts',(99.5720896931292,2.14621056620963,0.50158696302041));
#20607=CARTESIAN_POINT('Ctrl Pts',(99.5713469061111,2.14933181663506,0.488038963727046));
#20608=CARTESIAN_POINT('Ctrl Pts',(99.5693992846938,2.1572222753737,0.45224510658668));
#20609=CARTESIAN_POINT('Ctrl Pts',(99.5682013655059,2.16177565547391,0.429953076746752));
#20610=CARTESIAN_POINT('Ctrl Pts',(99.5627707661021,2.18101627712602,0.327707053304118));
#20611=CARTESIAN_POINT('Ctrl Pts',(99.5586674260433,2.19161907236155,0.247045592254468));
#20612=CARTESIAN_POINT('Ctrl Pts',(99.5478517573652,2.20809860871596,0.028835408900884));
#20613=CARTESIAN_POINT('Ctrl Pts',(99.5413358282679,2.20559643271538,-0.108969296794327));
#20614=CARTESIAN_POINT('Ctrl Pts',(99.5308421279577,2.18173498617732,-0.321731440484667));
#20615=CARTESIAN_POINT('Ctrl Pts',(99.5270215361818,2.16924261694441,-0.397319970989235));
#20616=CARTESIAN_POINT('Ctrl Pts',(99.5220360869912,2.14881799093012,-0.490459572740548));
#20617=CARTESIAN_POINT('Ctrl Pts',(99.5210424522371,2.14455692231191,-0.508768032697666));
#20618=CARTESIAN_POINT('Ctrl Pts',(99.5195538313485,2.13790748154261,-0.535769362885681));
#20619=CARTESIAN_POINT('Ctrl Pts',(99.5190685437826,2.13569901322567,-0.544506133096103));
#20620=CARTESIAN_POINT('Ctrl Pts',(99.5182333465882,2.13183059202771,-0.559424067266786));
#20621=CARTESIAN_POINT('Ctrl Pts',(99.5178849587174,2.13019720260091,-0.565611913809608));
#20622=CARTESIAN_POINT('Ctrl Pts',(99.5170825168608,2.12639032416238,-0.579783275036138));
#20623=CARTESIAN_POINT('Ctrl Pts',(99.5166274553018,2.12419886150868,-0.587761557840866));
#20624=CARTESIAN_POINT('Ctrl Pts',(99.5153542301126,2.1179753360343,-0.609929571303033));
#20625=CARTESIAN_POINT('Ctrl Pts',(99.51453076822,2.11384572960998,-0.624091189950439));
#20626=CARTESIAN_POINT('Ctrl Pts',(99.5094516320481,2.08771792367807,-0.710455490058696));
#20627=CARTESIAN_POINT('Ctrl Pts',(99.5050275497542,2.06216643813587,-0.781524596915789));
#20628=CARTESIAN_POINT('Ctrl Pts',(99.4927915936766,1.98275900860031,-0.971197098370056));
#20629=CARTESIAN_POINT('Ctrl Pts',(99.4848859747996,1.92195472645178,-1.08657711892708));
#20630=CARTESIAN_POINT('Ctrl Pts',(99.4715815235569,1.79954400286778,-1.27607354707506));
#20631=CARTESIAN_POINT('Ctrl Pts',(99.4660857781109,1.74260860657966,-1.35279017281286));
#20632=CARTESIAN_POINT('Ctrl Pts',(99.4595053801944,1.66602298811145,-1.44309059293132));
#20633=CARTESIAN_POINT('Ctrl Pts',(99.4582405833393,1.65090054788253,-1.46036656141583));
#20634=CARTESIAN_POINT('Ctrl Pts',(99.456226049229,1.62616902483565,-1.48774477199782));
#20635=CARTESIAN_POINT('Ctrl Pts',(99.4554692888896,1.61672951037853,-1.49799729865023));
#20636=CARTESIAN_POINT('Ctrl Pts',(99.4540321275149,1.59851979729358,-1.51740275432467));
#20637=CARTESIAN_POINT('Ctrl Pts',(99.4533510398692,1.58976666534688,-1.52657086970617));
#20638=CARTESIAN_POINT('Ctrl Pts',(99.4518068856642,1.56964290794713,-1.54728788009442));
#20639=CARTESIAN_POINT('Ctrl Pts',(99.4509460232576,1.55822294587838,-1.55878796257449));
#20640=CARTESIAN_POINT('Ctrl Pts',(99.4486699080619,1.52750173988276,-1.58904968357083));
#20641=CARTESIAN_POINT('Ctrl Pts',(99.4472644233843,1.50798161170357,-1.60758576842676));
#20642=CARTESIAN_POINT('Ctrl Pts',(99.4371017744592,1.3629690998057,-1.74032178334487));
#20643=CARTESIAN_POINT('Ctrl Pts',(99.4289805642944,1.22500446514931,-1.84004715217366));
#20644=CARTESIAN_POINT('Ctrl Pts',(99.4151158764487,0.975127467042809,-1.97999080591622));
#20645=CARTESIAN_POINT('Ctrl Pts',(99.4094249065928,0.868941510257868,-2.02883507148214));
#20646=CARTESIAN_POINT('Ctrl Pts',(99.4024281938829,0.743835251543739,-2.0747530252302));
#20647=CARTESIAN_POINT('Ctrl Pts',(99.4015488858329,0.728204136935626,-2.08029077281181));
#20648=CARTESIAN_POINT('Ctrl Pts',(99.4002002192111,0.704404071468602,-2.08842149092379));
#20649=CARTESIAN_POINT('Ctrl Pts',(99.3997381165754,0.696279703642808,-2.09114418176732));
#20650=CARTESIAN_POINT('Ctrl Pts',(99.3988889887552,0.681412270372782,-2.09603040677843));
#20651=CARTESIAN_POINT('Ctrl Pts',(99.398502838266,0.674674410855502,-2.09820889900794));
#20652=CARTESIAN_POINT('Ctrl Pts',(99.3976206321168,0.659333266612976,-2.10308747985607));
#20653=CARTESIAN_POINT('Ctrl Pts',(99.3971234397088,0.650723865382452,-2.1057672591113));
#20654=CARTESIAN_POINT('Ctrl Pts',(99.3955793774784,0.624089670264132,-2.1138785390297));
#20655=CARTESIAN_POINT('Ctrl Pts',(99.3945229962931,0.60601199571494,-2.11913185220807));
#20656=CARTESIAN_POINT('Ctrl Pts',(99.3849132823995,0.442608285957629,-2.16435464434205));
#20657=CARTESIAN_POINT('Ctrl Pts',(99.3757467496148,0.293615410072287,-2.18954746617142));
#20658=CARTESIAN_POINT('Ctrl Pts',(99.3595079860396,0.0231141936463182,
-2.20716342558941));
#20659=CARTESIAN_POINT('Ctrl Pts',(99.3524078570309,-0.097451368274999,
-2.2051336192787));
#20660=CARTESIAN_POINT('Ctrl Pts',(99.3434857745974,-0.25447353019184,-2.18957932716182));
#20661=CARTESIAN_POINT('Ctrl Pts',(99.3413994803973,-0.291588307739401,
-2.18494643120161));
#20662=CARTESIAN_POINT('Ctrl Pts',(99.3384192771659,-0.345170152402561,
-2.17686826236887));
#20663=CARTESIAN_POINT('Ctrl Pts',(99.3375019289786,-0.361742573993451,
-2.17417575140373));
#20664=CARTESIAN_POINT('Ctrl Pts',(99.335899682225,-0.390821999819147,-2.16910953265496));
#20665=CARTESIAN_POINT('Ctrl Pts',(99.335212265111,-0.403342074745187,-2.16681636979938));
#20666=CARTESIAN_POINT('Ctrl Pts',(99.3337859539989,-0.429407694041341,
-2.16180846973057));
#20667=CARTESIAN_POINT('Ctrl Pts',(99.333047703711,-0.442949019142456,-2.15907457162863));
#20668=CARTESIAN_POINT('Ctrl Pts',(99.3311255769567,-0.478328193106123,
-2.15158490610087));
#20669=CARTESIAN_POINT('Ctrl Pts',(99.3299482848148,-0.500121258145158,
-2.14662391770354));
#20670=CARTESIAN_POINT('Ctrl Pts',(99.3247868326121,-0.59613760328773,-2.1232250487795));
#20671=CARTESIAN_POINT('Ctrl Pts',(99.320915995835,-0.669450502817471,-2.10126204626879));
#20672=CARTESIAN_POINT('Ctrl Pts',(99.3101837649922,-0.873322604034533,
-2.02842919451307));
#20673=CARTESIAN_POINT('Ctrl Pts',(99.303549796962,-1.00037455557691,-1.96887464541769));
#20674=CARTESIAN_POINT('Ctrl Pts',(99.2928327941451,-1.18887844144873,-1.85752902671119));
#20675=CARTESIAN_POINT('Ctrl Pts',(99.2889014011253,-1.25462763201251,-1.81376773803157));
#20676=CARTESIAN_POINT('Ctrl Pts',(99.2837807718046,-1.33316726324129,-1.75517654410181));
#20677=CARTESIAN_POINT('Ctrl Pts',(99.2827731359424,-1.34830310705554,-1.74357630628449));
#20678=CARTESIAN_POINT('Ctrl Pts',(99.281267386904,-1.3704091346105,-1.72617408912786));
#20679=CARTESIAN_POINT('Ctrl Pts',(99.2807792906664,-1.37749746539367,-1.72052285924018));
#20680=CARTESIAN_POINT('Ctrl Pts',(99.2799408277803,-1.38953696003429,-1.71080218288318));
#20681=CARTESIAN_POINT('Ctrl Pts',(99.2795920142805,-1.39450554428029,-1.7067546274031));
#20682=CARTESIAN_POINT('Ctrl Pts',(99.2787907594888,-1.40582647840209,-1.69744982244778));
#20683=CARTESIAN_POINT('Ctrl Pts',(99.2783373331855,-1.41216689311513,-1.69217866921574));
#20684=CARTESIAN_POINT('Ctrl Pts',(99.2770738312634,-1.42965802081289,-1.67747051803249));
#20685=CARTESIAN_POINT('Ctrl Pts',(99.2762585891127,-1.44074451834345,-1.6679582143597));
#20686=CARTESIAN_POINT('Ctrl Pts',(99.2713608120757,-1.50623281984018,-1.61062867296098));
#20687=CARTESIAN_POINT('Ctrl Pts',(99.2671231367401,-1.55834096298168,-1.56026717074403));
#20688=CARTESIAN_POINT('Ctrl Pts',(99.2549147374783,-1.69885828811758,-1.41038783220531));
#20689=CARTESIAN_POINT('Ctrl Pts',(99.246829017045,-1.78087797261919,-1.30529296890879));
#20690=CARTESIAN_POINT('Ctrl Pts',(99.2333319654,-1.90478768401034,-1.11291306086762));
#20691=CARTESIAN_POINT('Ctrl Pts',(99.2278145692006,-1.95135609746673,-1.02907954563236));
#20692=CARTESIAN_POINT('Ctrl Pts',(99.2212119786078,-2.00215682157566,-0.921690084339665));
#20693=CARTESIAN_POINT('Ctrl Pts',(99.2199453502669,-2.01166234687263,-0.900754799320084));
#20694=CARTESIAN_POINT('Ctrl Pts',(99.2179282217553,-2.02640652601918,-0.866883605633653));
#20695=CARTESIAN_POINT('Ctrl Pts',(99.2171706810794,-2.03185275045717,-0.854040401531174));
#20696=CARTESIAN_POINT('Ctrl Pts',(99.2157322232877,-2.04201775899832,-0.829421707925496));
#20697=CARTESIAN_POINT('Ctrl Pts',(99.2150506169327,-2.04675751725235,-0.817655534157717));
#20698=CARTESIAN_POINT('Ctrl Pts',(99.2135055197959,-2.05732375478196,-0.790757772653534));
#20699=CARTESIAN_POINT('Ctrl Pts',(99.2126442316379,-2.06308540058328,-0.775601402710669));
#20700=CARTESIAN_POINT('Ctrl Pts',(99.2103674460596,-2.07796668217005,-0.735115728443673));
#20701=CARTESIAN_POINT('Ctrl Pts',(99.2089617078953,-2.08679053812886,-0.709680208431343));
#20702=CARTESIAN_POINT('Ctrl Pts',(99.1988018417313,-2.14778940594839,-0.522860037950963));
#20703=CARTESIAN_POINT('Ctrl Pts',(99.1906825728083,-2.18164661973111,-0.356096556944589));
#20704=CARTESIAN_POINT('Ctrl Pts',(99.1767829080258,-2.20601560498352,-0.0700547651467955));
#20705=CARTESIAN_POINT('Ctrl Pts',(99.1710545462894,-2.20661340458709,0.0475770978464523));
#20706=CARTESIAN_POINT('Ctrl Pts',(99.1640363669841,-2.19663506640115,0.180748442571447));
#20707=CARTESIAN_POINT('Ctrl Pts',(99.1631813709976,-2.19525502677082,0.196801808456324));
#20708=CARTESIAN_POINT('Ctrl Pts',(99.1618623298947,-2.19288063577909,0.221274394690537));
#20709=CARTESIAN_POINT('Ctrl Pts',(99.1614050523952,-2.19201348431048,0.229705725366978));
#20710=CARTESIAN_POINT('Ctrl Pts',(99.1605601976457,-2.19033163130044,0.245180793585658));
#20711=CARTESIAN_POINT('Ctrl Pts',(99.160173429736,-2.18953154718281,0.252225844131779));
#20712=CARTESIAN_POINT('Ctrl Pts',(99.1592837022149,-2.18762229695979,0.268343484563493));
#20713=CARTESIAN_POINT('Ctrl Pts',(99.1587795265824,-2.18649068291347,0.277413098639144));
#20714=CARTESIAN_POINT('Ctrl Pts',(99.1571916195139,-2.18277069590441,0.305790062629107));
#20715=CARTESIAN_POINT('Ctrl Pts',(99.1560976103145,-2.17998280893129,0.325069796837474));
#20716=CARTESIAN_POINT('Ctrl Pts',(99.1468469086964,-2.15451272359991,0.486107664511512));
#20717=CARTESIAN_POINT('Ctrl Pts',(99.1381376724428,-2.11828658929199,0.625366029687957));
#20718=CARTESIAN_POINT('Ctrl Pts',(99.1236133749904,-2.03475895023049,0.852704278170789));
#20719=CARTESIAN_POINT('Ctrl Pts',(99.117755606344,-1.99455432184662,0.942923458206203));
#20720=CARTESIAN_POINT('Ctrl Pts',(99.1087284352821,-1.92129838437821,1.08148029920268));
#20721=CARTESIAN_POINT('Ctrl Pts',(99.1054466027748,-1.89214124788498,1.13171970782923));
#20722=CARTESIAN_POINT('Ctrl Pts',(99.1011428327917,-1.8504478453537,1.19743437449569));
#20723=CARTESIAN_POINT('Ctrl Pts',(99.1000585745337,-1.83963974155745,1.2139736268965));
#20724=CARTESIAN_POINT('Ctrl Pts',(99.0982603048778,-1.82120646433082,1.24136977684593));
#20725=CARTESIAN_POINT('Ctrl Pts',(99.0975417738708,-1.81370318082044,1.25230694769892));
#20726=CARTESIAN_POINT('Ctrl Pts',(99.09613435482,-1.79873561743709,1.27370771933775));
#20727=CARTESIAN_POINT('Ctrl Pts',(99.0954452661879,-1.79127764125888,1.28417506490551));
#20728=CARTESIAN_POINT('Ctrl Pts',(99.0937821950766,-1.7729657063493,1.3094061060183));
#20729=CARTESIAN_POINT('Ctrl Pts',(99.092811873513,-1.76201827139775,1.32410097227892));
#20730=CARTESIAN_POINT('Ctrl Pts',(99.0895380501984,-1.72419963885128,1.37356559870361));
#20731=CARTESIAN_POINT('Ctrl Pts',(99.0872681817162,-1.69647166083457,1.40766867156201));
#20732=CARTESIAN_POINT('Ctrl Pts',(99.0765884854177,-1.55923038431939,1.56651351028985));
#20733=CARTESIAN_POINT('Ctrl Pts',(99.0687159327872,-1.43688426599198,1.67944314635297));
#20734=CARTESIAN_POINT('Ctrl Pts',(99.0561576897297,-1.22866877651398,1.8320717624898));
#20735=CARTESIAN_POINT('Ctrl Pts',(99.0516116482838,-1.15098080309927,1.88184855655554));
#20736=CARTESIAN_POINT('Ctrl Pts',(99.0457394544012,-1.05250742363309,1.93655976450964));
#20737=CARTESIAN_POINT('Ctrl Pts',(99.0446591073866,-1.03446419689044,1.94625778467098));
#20738=CARTESIAN_POINT('Ctrl Pts',(99.0430653062757,-1.00801449624914,1.96000248297032));
#20739=CARTESIAN_POINT('Ctrl Pts',(99.0425636380636,-0.999712865630564,
1.96424976462608));
#20740=CARTESIAN_POINT('Ctrl Pts',(99.0416773830374,-0.985095607952631,
1.97161158148471));
#20741=CARTESIAN_POINT('Ctrl Pts',(99.0412942039352,-0.978791649243712,
1.97474871592414));
#20742=CARTESIAN_POINT('Ctrl Pts',(99.0404543305542,-0.965010640260082,
1.98152456600385));
#20743=CARTESIAN_POINT('Ctrl Pts',(99.039996942569,-0.957528111401297,1.98515114102489));
#20744=CARTESIAN_POINT('Ctrl Pts',(99.0387118491751,-0.936561190004355,
1.99516710842875));
#20745=CARTESIAN_POINT('Ctrl Pts',(99.0378786994663,-0.923032412544451,
2.00146191413888));
#20746=CARTESIAN_POINT('Ctrl Pts',(99.0322980937603,-0.832754303357346,
2.0423574425992));
#20747=CARTESIAN_POINT('Ctrl Pts',(99.0273411984425,-0.754146644769432,
2.07267071416765));
#20748=CARTESIAN_POINT('Ctrl Pts',(99.0203784033333,-0.643087408717639,
2.10834276080852));
#20749=CARTESIAN_POINT('Ctrl Pts',(99.0184303972988,-0.611953003980711,
2.11758921622595));
#20750=CARTESIAN_POINT('Ctrl Pts',(99.0109245910529,-0.491393010644367,
2.15051279165374));
#20751=CARTESIAN_POINT('Ctrl Pts',(99.0053620417862,-0.400710246579317,
2.16924068346033));
#20752=CARTESIAN_POINT('Ctrl Pts',(98.9963212997439,-0.248652954517391,
2.19077996224226));
#20753=CARTESIAN_POINT('Ctrl Pts',(98.9927797481123,-0.187856803092223,
2.19682859171664));
#20754=CARTESIAN_POINT('Ctrl Pts',(98.9869169066235,-0.0848271257078374,
2.20276985289966));
#20755=CARTESIAN_POINT('Ctrl Pts',(98.9845588362986,-0.0427074822583268,
2.20398890193156));
#20756=CARTESIAN_POINT('Ctrl Pts',(98.9822274881864,-0.000384419624161417,
2.20399997485622));
#20757=CARTESIAN_POINT('Ctrl Pts',(98.982216901173,-0.000192209799753219,
2.204));
#20758=CARTESIAN_POINT('Ctrl Pts',(98.9822063149447,-3.98666500548274E-14,
2.204));
#20759=CARTESIAN_POINT('Ctrl Pts',(98.8779717715633,2.72446158072696E-13,
2.204));
#20760=CARTESIAN_POINT('Ctrl Pts',(98.8779819576879,-0.000195548552893731,
2.204));
#20761=CARTESIAN_POINT('Ctrl Pts',(98.8779921430541,-0.000391097255348482,
2.20399997397511));
#20762=CARTESIAN_POINT('Ctrl Pts',(98.8842321210603,-0.120201351076194,
2.20396808367526));
#20763=CARTESIAN_POINT('Ctrl Pts',(98.8901497521798,-0.239620005710135,
2.19419922271989));
#20764=CARTESIAN_POINT('Ctrl Pts',(98.8996566185453,-0.432634550292262,
2.16245589655867));
#20765=CARTESIAN_POINT('Ctrl Pts',(98.903304935187,-0.506913965546811,2.14625867285324));
#20766=CARTESIAN_POINT('Ctrl Pts',(98.9119661043065,-0.678794290353091,
2.09935638758593));
#20767=CARTESIAN_POINT('Ctrl Pts',(98.9170040688667,-0.775380083419822,
2.06563312797774));
#20768=CARTESIAN_POINT('Ctrl Pts',(98.9231841836035,-0.883295505522182,
2.019316246659));
#20769=CARTESIAN_POINT('Ctrl Pts',(98.9239950325058,-0.897260777253245,
2.01314980216912));
#20770=CARTESIAN_POINT('Ctrl Pts',(98.9252673157792,-0.918846802374575,
2.00334914883852));
#20771=CARTESIAN_POINT('Ctrl Pts',(98.92572290691,-0.926512888221899,1.9998152718533));
#20772=CARTESIAN_POINT('Ctrl Pts',(98.9265709205397,-0.940659383164747,
1.99319528479629));
#20773=CARTESIAN_POINT('Ctrl Pts',(98.9269626037561,-0.947145236154838,
1.9901214574628));
#20774=CARTESIAN_POINT('Ctrl Pts',(98.9278724512557,-0.962101596949523,
1.98294354646419));
#20775=CARTESIAN_POINT('Ctrl Pts',(98.9283919741667,-0.970560919166227,
1.9788168401509));
#20776=CARTESIAN_POINT('Ctrl Pts',(98.9300616107466,-0.997501306033836,
1.96546022223597));
#20777=CARTESIAN_POINT('Ctrl Pts',(98.9312234054895,-1.01587863170852,1.95602486780533));
#20778=CARTESIAN_POINT('Ctrl Pts',(98.9376892954594,-1.11632936092291,1.90265368074079));
#20779=CARTESIAN_POINT('Ctrl Pts',(98.9432226407972,-1.1956824255753,1.85381309047381));
#20780=CARTESIAN_POINT('Ctrl Pts',(98.9589291016104,-1.40966150824606,1.70264552509731));
#20781=CARTESIAN_POINT('Ctrl Pts',(98.9691119368599,-1.53598059806489,1.5896308996929));
#20782=CARTESIAN_POINT('Ctrl Pts',(98.9810240701708,-1.67524180850678,1.43277538891879));
#20783=CARTESIAN_POINT('Ctrl Pts',(98.9833079878426,-1.70147696633201,1.40151948841479));
#20784=CARTESIAN_POINT('Ctrl Pts',(98.9864485502119,-1.73688220248456,1.35687798770791));
#20785=CARTESIAN_POINT('Ctrl Pts',(98.9873345971617,-1.74679413978557,1.34409371390439));
#20786=CARTESIAN_POINT('Ctrl Pts',(98.9888647915214,-1.76377424421074,1.32168789717984));
#20787=CARTESIAN_POINT('Ctrl Pts',(98.9895114474958,-1.77090655545369,1.31211602452172));
#20788=CARTESIAN_POINT('Ctrl Pts',(98.9908582271073,-1.78566753173705,1.29196653580043));
#20789=CARTESIAN_POINT('Ctrl Pts',(98.9915577371709,-1.79328080062611,1.28137818138705));
#20790=CARTESIAN_POINT('Ctrl Pts',(98.9932202075996,-1.81124245128677,1.25592389799731));
#20791=CARTESIAN_POINT('Ctrl Pts',(98.9941797726967,-1.82150252313242,1.24099663149863));
#20792=CARTESIAN_POINT('Ctrl Pts',(98.9974966396391,-1.8565740887023,1.18859922961264));
#20793=CARTESIAN_POINT('Ctrl Pts',(98.9998182233471,-1.88042351248254,1.15049695738275));
#20794=CARTESIAN_POINT('Ctrl Pts',(99.0054981585673,-1.93675014652145,1.05407191048516));
#20795=CARTESIAN_POINT('Ctrl Pts',(99.0088097243281,-1.96777520661731,0.994952393247454));
#20796=CARTESIAN_POINT('Ctrl Pts',(99.0188405630806,-2.0546537273671,0.809384478300428));
#20797=CARTESIAN_POINT('Ctrl Pts',(99.0253749846822,-2.10133742770108,0.679031032695808));
#20798=CARTESIAN_POINT('Ctrl Pts',(99.0353464024369,-2.15103009635578,0.48437818857596));
#20799=CARTESIAN_POINT('Ctrl Pts',(99.0385261031426,-2.16394569212151,0.422954470608338));
#20800=CARTESIAN_POINT('Ctrl Pts',(99.0425836191876,-2.17654692845008,0.347074506286445));
#20801=CARTESIAN_POINT('Ctrl Pts',(99.0433384786084,-2.17873572578328,0.333058344683618));
#20802=CARTESIAN_POINT('Ctrl Pts',(99.0445411329203,-2.18197573696531,0.310910116796425));
#20803=CARTESIAN_POINT('Ctrl Pts',(99.0449840590829,-2.18311716929175,0.302791410289721));
#20804=CARTESIAN_POINT('Ctrl Pts',(99.0458220622702,-2.18517895953167,0.287508413564723));
#20805=CARTESIAN_POINT('Ctrl Pts',(99.0462165783078,-2.18610942786841,0.280345745517549));
#20806=CARTESIAN_POINT('Ctrl Pts',(99.0471516433973,-2.18822079192894,0.263442661046369));
#20807=CARTESIAN_POINT('Ctrl Pts',(99.0476938144531,-2.18937187214884,0.253698773852814));
#20808=CARTESIAN_POINT('Ctrl Pts',(99.0495145460236,-2.19299657066233,0.221151843992155));
#20809=CARTESIAN_POINT('Ctrl Pts',(99.0508078202551,-2.19517920330723,0.19831862700156));
#20810=CARTESIAN_POINT('Ctrl Pts',(99.0540072349077,-2.19964503383976,0.142399042751306));
#20811=CARTESIAN_POINT('Ctrl Pts',(99.0559290812575,-2.20153850050353,0.109287679370813));
#20812=CARTESIAN_POINT('Ctrl Pts',(99.0641816120771,-2.20640466801385,-0.0314732378845199));
#20813=CARTESIAN_POINT('Ctrl Pts',(99.0706952879823,-2.20223274059584,-0.139218919484558));
#20814=CARTESIAN_POINT('Ctrl Pts',(99.0851133559994,-2.17536224171632,-0.378235751407745));
#20815=CARTESIAN_POINT('Ctrl Pts',(99.0929473820982,-2.14861512900064,-0.508650222839978));
#20816=CARTESIAN_POINT('Ctrl Pts',(99.102166015032,-2.10128187895847,-0.665734914531923));
#20817=CARTESIAN_POINT('Ctrl Pts',(99.1038983440931,-2.09165165097905,-0.69540062029428));
#20818=CARTESIAN_POINT('Ctrl Pts',(99.1064851959957,-2.07615150258665,-0.739908849775325));
#20819=CARTESIAN_POINT('Ctrl Pts',(99.1073548213281,-2.07074497912298,-0.754907555892946));
#20820=CARTESIAN_POINT('Ctrl Pts',(99.1089094067156,-2.06072749829178,-0.781780263840039));
#20821=CARTESIAN_POINT('Ctrl Pts',(99.109596293608,-2.05617549147496,-0.793675349811464));
#20822=CARTESIAN_POINT('Ctrl Pts',(99.1110582322353,-2.04621836449682,-0.819034105401334));
#20823=CARTESIAN_POINT('Ctrl Pts',(99.1118322246287,-2.04078288271679,-0.832485255348903));
#20824=CARTESIAN_POINT('Ctrl Pts',(99.1139373156913,-2.02555278680329,-0.86912927747891));
#20825=CARTESIAN_POINT('Ctrl Pts',(99.1152594034335,-2.01549282940701,-0.892209905891794));
#20826=CARTESIAN_POINT('Ctrl Pts',(99.1244799731463,-1.94188981603775,-1.05347612791501));
#20827=CARTESIAN_POINT('Ctrl Pts',(99.1318691014482,-1.86458794870026,-1.18493281352967));
#20828=CARTESIAN_POINT('Ctrl Pts',(99.1458398045079,-1.69312843659415,-1.41763293459058));
#20829=CARTESIAN_POINT('Ctrl Pts',(99.1524119494182,-1.60181207777976,-1.52005152776948));
#20830=CARTESIAN_POINT('Ctrl Pts',(99.1605947889176,-1.48701358716537,-1.62689999990013));
#20831=CARTESIAN_POINT('Ctrl Pts',(99.1616464037074,-1.47224536783317,-1.64027636091257));
#20832=CARTESIAN_POINT('Ctrl Pts',(99.1632083426155,-1.45033801598461,-1.65958480320958));
#20833=CARTESIAN_POINT('Ctrl Pts',(99.1637076312617,-1.44333914665913,-1.66567529281758));
#20834=CARTESIAN_POINT('Ctrl Pts',(99.1645983681987,-1.43086618238342,-1.67639175945168));
#20835=CARTESIAN_POINT('Ctrl Pts',(99.1649885095893,-1.42540769294651,-1.68103547555347));
#20836=CARTESIAN_POINT('Ctrl Pts',(99.1658478541629,-1.41339597419302,-1.69115366830288));
#20837=CARTESIAN_POINT('Ctrl Pts',(99.1663178239071,-1.406833633168,-1.69661664298097));
#20838=CARTESIAN_POINT('Ctrl Pts',(99.1676851706642,-1.38775448027841,-1.71231273126592));
#20839=CARTESIAN_POINT('Ctrl Pts',(99.1685892007942,-1.3751568593507,-1.72244621630854));
#20840=CARTESIAN_POINT('Ctrl Pts',(99.1765817214468,-1.26380584234128,-1.81001641985096));
#20841=CARTESIAN_POINT('Ctrl Pts',(99.1841231591728,-1.15872518919438,-1.87901975974689));
#20842=CARTESIAN_POINT('Ctrl Pts',(99.2012714431274,-0.907653207599422,
-2.01478731211538));
#20843=CARTESIAN_POINT('Ctrl Pts',(99.210799976273,-0.75906405892106,-2.07534069296284));
#20844=CARTESIAN_POINT('Ctrl Pts',(99.2213374367414,-0.578569263933788,
-2.12688534314843));
#20845=CARTESIAN_POINT('Ctrl Pts',(99.2228770172868,-0.551785818500878,
-2.13399066658404));
#20846=CARTESIAN_POINT('Ctrl Pts',(99.2253087049501,-0.508829510245894,
-2.1445235959848));
#20847=CARTESIAN_POINT('Ctrl Pts',(99.2262111736437,-0.492740372365689,
-2.14827741938747));
#20848=CARTESIAN_POINT('Ctrl Pts',(99.2278043178493,-0.46408128644873,-2.15462507986063));
#20849=CARTESIAN_POINT('Ctrl Pts',(99.2284972652143,-0.451528165025448,
-2.15729066217659));
#20850=CARTESIAN_POINT('Ctrl Pts',(99.2299400761059,-0.425210908550469,
-2.16263919968189));
#20851=CARTESIAN_POINT('Ctrl Pts',(99.2306892282524,-0.41144297862788,-2.16530074413299));
#20852=CARTESIAN_POINT('Ctrl Pts',(99.2326514265378,-0.375117604198007,
-2.17196399415345));
#20853=CARTESIAN_POINT('Ctrl Pts',(99.2338574720032,-0.35252124637108,-2.17574576451316));
#20854=CARTESIAN_POINT('Ctrl Pts',(99.2398629922906,-0.238735833485533,
-2.19296986908662));
#20855=CARTESIAN_POINT('Ctrl Pts',(99.2444916252348,-0.146821960262342,
-2.20103552636029));
#20856=CARTESIAN_POINT('Ctrl Pts',(99.2535541043797,0.0374940970157028,
-2.20560848221647));
#20857=CARTESIAN_POINT('Ctrl Pts',(99.2579794673787,0.12970755991788,-2.2021105504077));
#20858=CARTESIAN_POINT('Ctrl Pts',(99.2639834222332,0.253022134079523,-2.18965841913081));
#20859=CARTESIAN_POINT('Ctrl Pts',(99.2655261100552,0.284540510739411,-2.18578609166718));
#20860=CARTESIAN_POINT('Ctrl Pts',(99.2712230416771,0.399692601715817,-2.16910567812424));
#20861=CARTESIAN_POINT('Ctrl Pts',(99.2754437726786,0.482645989649669,-2.15216721563663));
#20862=CARTESIAN_POINT('Ctrl Pts',(99.2806886967422,0.578937725767128,-2.12665768714003));
#20863=CARTESIAN_POINT('Ctrl Pts',(99.2814871561207,0.593423439896998,-2.12266116113004));
#20864=CARTESIAN_POINT('Ctrl Pts',(99.2827440493808,0.615929641385201,-2.11620344938766));
#20865=CARTESIAN_POINT('Ctrl Pts',(99.2831968624445,0.623979118265158,-2.11384399083369));
#20866=CARTESIAN_POINT('Ctrl Pts',(99.2840388188358,0.638832492234408,-2.10939794549622));
#20867=CARTESIAN_POINT('Ctrl Pts',(99.2844272230258,0.64563998150957,-2.10732428810101));
#20868=CARTESIAN_POINT('Ctrl Pts',(99.2853358729685,0.66146378946655,-2.10242026217501));
#20869=CARTESIAN_POINT('Ctrl Pts',(99.2858575381223,0.670472045502456,-2.09956484373857));
#20870=CARTESIAN_POINT('Ctrl Pts',(99.2875412215263,0.699314028067557,-2.09021802805107));
#20871=CARTESIAN_POINT('Ctrl Pts',(99.2887151898155,0.719073464730478,-2.08350301228916));
#20872=CARTESIAN_POINT('Ctrl Pts',(99.295316449121,0.828450962499218,-2.04459113268242));
#20873=CARTESIAN_POINT('Ctrl Pts',(99.3009828637042,0.915998318586846,-2.00689512132065));
#20874=CARTESIAN_POINT('Ctrl Pts',(99.3172181314714,1.15717691270074,-1.88397276347889));
#20875=CARTESIAN_POINT('Ctrl Pts',(99.3277801425298,1.30347842475317,-1.7858819131866));
#20876=CARTESIAN_POINT('Ctrl Pts',(99.3396657381627,1.46319571246208,-1.64860662951125));
#20877=CARTESIAN_POINT('Ctrl Pts',(99.341619693369,1.4892395080735,-1.62511888747566));
#20878=CARTESIAN_POINT('Ctrl Pts',(99.3444567846536,1.52672317447922,-1.58965584656953));
#20879=CARTESIAN_POINT('Ctrl Pts',(99.3453599997491,1.53860545699172,-1.57815798663196));
#20880=CARTESIAN_POINT('Ctrl Pts',(99.3469539204563,1.55947877360995,-1.55750012597765));
#20881=CARTESIAN_POINT('Ctrl Pts',(99.3476469072359,1.56852119369887,-1.54839334873592));
#20882=CARTESIAN_POINT('Ctrl Pts',(99.3490892662852,1.58726989598803,-1.52917841962006));
#20883=CARTESIAN_POINT('Ctrl Pts',(99.3498379329853,1.5969603733939,-1.51905560792957));
#20884=CARTESIAN_POINT('Ctrl Pts',(99.3517976503572,1.62221077610405,-1.49216998298958));
#20885=CARTESIAN_POINT('Ctrl Pts',(99.3530017309911,1.63760767651869,-1.47525598113192));
#20886=CARTESIAN_POINT('Ctrl Pts',(99.358976117133,1.71334395391468,-1.38941010806373));
#20887=CARTESIAN_POINT('Ctrl Pts',(99.363577808431,1.76961037487185,-1.31700017842805));
#20888=CARTESIAN_POINT('Ctrl Pts',(99.3726313178278,1.87331675995762,-1.16484322800207));
#20889=CARTESIAN_POINT('Ctrl Pts',(99.3770725948651,1.92055784933156,-1.08518815601464));
#20890=CARTESIAN_POINT('Ctrl Pts',(99.3830480279422,1.97668631848116,-0.975335051929698));
#20891=CARTESIAN_POINT('Ctrl Pts',(99.3845462431251,1.9901411877012,-0.947578636071126));
#20892=CARTESIAN_POINT('Ctrl Pts',(99.3902522214846,2.03879171915261,-0.841605588752568));
#20893=CARTESIAN_POINT('Ctrl Pts',(99.3945274541168,2.06999107473806,-0.761646736059623));
#20894=CARTESIAN_POINT('Ctrl Pts',(99.3998348007729,2.10109643283176,-0.665760092312499));
#20895=CARTESIAN_POINT('Ctrl Pts',(99.4006348303378,2.10559558692611,-0.651390758415191));
#20896=CARTESIAN_POINT('Ctrl Pts',(99.4018936496943,2.11237312583705,-0.62894057343521));
#20897=CARTESIAN_POINT('Ctrl Pts',(99.4023467897566,2.11475324358211,-0.620890635859239));
#20898=CARTESIAN_POINT('Ctrl Pts',(99.4031890129687,2.11906576994465,-0.60599248641347));
#20899=CARTESIAN_POINT('Ctrl Pts',(99.4035773523723,2.12101107036898,-0.599148283538529));
#20900=CARTESIAN_POINT('Ctrl Pts',(99.4044853688258,2.12546003187099,-0.583202164515569));
#20901=CARTESIAN_POINT('Ctrl Pts',(99.4050064587185,2.12793838633418,-0.574093484588346));
#20902=CARTESIAN_POINT('Ctrl Pts',(99.4066862787295,2.13569264993574,-0.544854095496048));
#20903=CARTESIAN_POINT('Ctrl Pts',(99.4078568838098,2.14074183689371,-0.52466503972739));
#20904=CARTESIAN_POINT('Ctrl Pts',(99.4144201731322,2.16716039172308,-0.412293530731154));
#20905=CARTESIAN_POINT('Ctrl Pts',(99.4200491857681,2.1828601388763,-0.318886838354072));
#20906=CARTESIAN_POINT('Ctrl Pts',(99.4361336124783,2.21021298531451,-0.0520739424175816));
#20907=CARTESIAN_POINT('Ctrl Pts',(99.4465872133594,2.20745394026298,0.122138351323359));
#20908=CARTESIAN_POINT('Ctrl Pts',(99.4585115445208,2.17929807565128,0.331155146551179));
#20909=CARTESIAN_POINT('Ctrl Pts',(99.4605898495478,2.17338922909748,0.367944738699607));
#20910=CARTESIAN_POINT('Ctrl Pts',(99.4635562891413,2.16348856676216,0.42096488780234));
#20911=CARTESIAN_POINT('Ctrl Pts',(99.464467723569,2.16024071916095,0.437326276531178));
#20912=CARTESIAN_POINT('Ctrl Pts',(99.4660711257746,2.15416131875394,0.466229856064673));
#20913=CARTESIAN_POINT('Ctrl Pts',(99.4667654650416,2.151405198076,0.478786956148474));
#20914=CARTESIAN_POINT('Ctrl Pts',(99.4682057617156,2.14543025095464,0.504915394254023));
#20915=CARTESIAN_POINT('Ctrl Pts',(99.4689510653189,2.14219214557338,0.518481765128088));
#20916=CARTESIAN_POINT('Ctrl Pts',(99.4708911349949,2.13338026716489,0.553907475462395));
#20917=CARTESIAN_POINT('Ctrl Pts',(99.4720791932562,2.12759922226144,0.575713865483944));
#20918=CARTESIAN_POINT('Ctrl Pts',(99.4777977009217,2.09791120601089,0.68113684055803));
#20919=CARTESIAN_POINT('Ctrl Pts',(99.4821774472969,2.0694033087223,0.763381215537553));
#20920=CARTESIAN_POINT('Ctrl Pts',(99.4912235733024,1.99914849607456,0.932921154614271));
#20921=CARTESIAN_POINT('Ctrl Pts',(99.4958580202553,1.95636899547256,1.01958688724714));
#20922=CARTESIAN_POINT('Ctrl Pts',(99.5058109138713,1.85350152980109,1.19750692642425));
#20923=CARTESIAN_POINT('Ctrl Pts',(99.5111277827863,1.79204179445364,1.28766154482144));
#20924=CARTESIAN_POINT('Ctrl Pts',(99.5178745450657,1.71137199444857,1.38897242947922));
#20925=CARTESIAN_POINT('Ctrl Pts',(99.5189579953094,1.69834413657979,1.40487211067572));
#20926=CARTESIAN_POINT('Ctrl Pts',(99.5205606481797,1.67901355583851,1.42780199591138));
#20927=CARTESIAN_POINT('Ctrl Pts',(99.52106807592,1.67288466564146,1.4349780308815));
#20928=CARTESIAN_POINT('Ctrl Pts',(99.5219684751114,1.66199987406497,1.44755802557908));
#20929=CARTESIAN_POINT('Ctrl Pts',(99.5223600459261,1.65726330998197,1.45297836838577));
#20930=CARTESIAN_POINT('Ctrl Pts',(99.5231793752735,1.64734794823736,1.46421356525199));
#20931=CARTESIAN_POINT('Ctrl Pts',(99.5236074163515,1.64216494102976,1.47002412560153));
#20932=CARTESIAN_POINT('Ctrl Pts',(99.5247752621424,1.62801226807455,1.48572213813831));
#20933=CARTESIAN_POINT('Ctrl Pts',(99.5255192598734,1.61898352231481,1.49555560019222));
#20934=CARTESIAN_POINT('Ctrl Pts',(99.5272304205214,1.59817406593917,1.51781050192986));
#20935=CARTESIAN_POINT('Ctrl Pts',(99.5282012129174,1.58633693607812,1.5301778185648));
#20936=CARTESIAN_POINT('Ctrl Pts',(99.5312920955836,1.54850703200064,1.5687913870468));
#20937=CARTESIAN_POINT('Ctrl Pts',(99.5334409204209,1.52199870138607,1.59452191586549));
#20938=CARTESIAN_POINT('Ctrl Pts',(99.5433514506028,1.39819764812139,1.70878966785774));
#20939=CARTESIAN_POINT('Ctrl Pts',(99.5513545933414,1.2937457944548,1.78917329854906));
#20940=CARTESIAN_POINT('Ctrl Pts',(99.5659789050298,1.0862732507725,1.92111907342853));
#20941=CARTESIAN_POINT('Ctrl Pts',(99.5726243078922,0.985159774363577,1.97488086049082));
#20942=CARTESIAN_POINT('Ctrl Pts',(99.5803630711005,0.857787132007931,2.03037465604049));
#20943=CARTESIAN_POINT('Ctrl Pts',(99.5817193351804,0.835092880834106,2.03981370648384));
#20944=CARTESIAN_POINT('Ctrl Pts',(99.5838489547668,0.798874975052813,2.05417176014373));
#20945=CARTESIAN_POINT('Ctrl Pts',(99.5846306781474,0.785453347338186,2.05934113222772));
#20946=CARTESIAN_POINT('Ctrl Pts',(99.5860285485871,0.761227520663636,2.06840046675538));
#20947=CARTESIAN_POINT('Ctrl Pts',(99.5866462688971,0.750441789841577,2.07233804097646));
#20948=CARTESIAN_POINT('Ctrl Pts',(99.5880924270923,0.725005104672771,2.08139964592174));
#20949=CARTESIAN_POINT('Ctrl Pts',(99.5889185159181,0.710329718981657,2.08645359280059));
#20950=CARTESIAN_POINT('Ctrl Pts',(99.5913304252522,0.667067653094773,2.10084293183861));
#20951=CARTESIAN_POINT('Ctrl Pts',(99.5929021761282,0.638341314950516,2.10974897988092));
#20952=CARTESIAN_POINT('Ctrl Pts',(99.6001030646095,0.504450129678244,2.14827412387405));
#20953=CARTESIAN_POINT('Ctrl Pts',(99.6054993738531,0.397352364815328,2.17063722383543));
#20954=CARTESIAN_POINT('Ctrl Pts',(99.6155366188792,0.192633336516848,2.19771779147581));
#20955=CARTESIAN_POINT('Ctrl Pts',(99.6201868564507,0.0955024069012108,
2.20407547326078));
#20956=CARTESIAN_POINT('Ctrl Pts',(99.6249543031017,-0.00172616788486746,
2.20399932403448));
#20957=CARTESIAN_POINT('Origin',(88.3562164250559,0.,0.));
#20958=CARTESIAN_POINT('',(90.9367078804582,1.77561363837197,-0.0475422940912709));
#20959=CARTESIAN_POINT('',(90.7899230490922,1.77530581490221,-0.0474953858958096));
#20960=CARTESIAN_POINT('',(88.3562164250559,1.77561363837197,-0.0475422940912398));
#20961=CARTESIAN_POINT('',(90.3498698986825,0.408169026503128,1.72871689651704));
#20962=CARTESIAN_POINT('Ctrl Pts',(90.9367078804582,1.77561363837197,-0.047542294091302));
#20963=CARTESIAN_POINT('Ctrl Pts',(90.9366940428792,1.77560821463806,-0.0477448601658868));
#20964=CARTESIAN_POINT('Ctrl Pts',(90.9366802071354,1.77560275623504,-0.0479474255107499));
#20965=CARTESIAN_POINT('Ctrl Pts',(90.9362063763554,1.77541461075793,-0.0548855493489321));
#20966=CARTESIAN_POINT('Ctrl Pts',(90.9357484215827,1.77519362986983,-0.0616201586282712));
#20967=CARTESIAN_POINT('Ctrl Pts',(90.9347807730013,1.77464311481225,-0.0759153772536121));
#20968=CARTESIAN_POINT('Ctrl Pts',(90.9342716652679,1.7743035754535,-0.0834754835775824));
#20969=CARTESIAN_POINT('Ctrl Pts',(90.932978732698,1.77331355919584,-0.102767374601682));
#20970=CARTESIAN_POINT('Ctrl Pts',(90.9321985825354,1.77259496333718,-0.114495532509192));
#20971=CARTESIAN_POINT('Ctrl Pts',(90.9288988399027,1.76903793233093,-0.164427403387343));
#20972=CARTESIAN_POINT('Ctrl Pts',(90.9264340184423,1.7650801781021,-0.202543892264564));
#20973=CARTESIAN_POINT('Ctrl Pts',(90.9192199515912,1.74966032069272,-0.315378249871152));
#20974=CARTESIAN_POINT('Ctrl Pts',(90.9145852724228,1.73465992769765,-0.389526819189099));
#20975=CARTESIAN_POINT('Ctrl Pts',(90.9028862768841,1.68503073000851,-0.573555756497857));
#20976=CARTESIAN_POINT('Ctrl Pts',(90.8958291998014,1.64436791040717,-0.681428770470135));
#20977=CARTESIAN_POINT('Ctrl Pts',(90.8868376996582,1.58270848745254,-0.806661080887335));
#20978=CARTESIAN_POINT('Ctrl Pts',(90.8852404037542,1.57139468000783,-0.828484713853723));
#20979=CARTESIAN_POINT('Ctrl Pts',(90.8825958288061,1.55210832501898,-0.863869763436651));
#20980=CARTESIAN_POINT('Ctrl Pts',(90.8815579058604,1.54440182282406,-0.877572905187356));
#20981=CARTESIAN_POINT('Ctrl Pts',(90.8796680124858,1.53013030331544,-0.902179163976264));
#20982=CARTESIAN_POINT('Ctrl Pts',(90.8788183517933,1.52362800428167,-0.913117560401485));
#20983=CARTESIAN_POINT('Ctrl Pts',(90.8769740530915,1.50933286759471,-0.936587477618503));
#20984=CARTESIAN_POINT('Ctrl Pts',(90.8759780003516,1.50150031625262,-0.949093560091067));
#20985=CARTESIAN_POINT('Ctrl Pts',(90.8731702394157,1.4791150708671,-0.983864903332042));
#20986=CARTESIAN_POINT('Ctrl Pts',(90.8713458334132,1.46421727113885,-1.00590217735028));
#20987=CARTESIAN_POINT('Ctrl Pts',(90.8632888076155,1.39693299671862,-1.10076783838728));
#20988=CARTESIAN_POINT('Ctrl Pts',(90.8568711993163,1.33957393479257,-1.16989277485529));
#20989=CARTESIAN_POINT('Ctrl Pts',(90.8432711798739,1.2096014097248,-1.3043788266945));
#20990=CARTESIAN_POINT('Ctrl Pts',(90.836092083392,1.13631510233555,-1.36869572950234));
#20991=CARTESIAN_POINT('Ctrl Pts',(90.8261172152295,1.02488054766708,-1.4513432959085));
#20992=CARTESIAN_POINT('Ctrl Pts',(90.8231783695936,0.990778324178097,-1.47483436488725));
#20993=CARTESIAN_POINT('Ctrl Pts',(90.819443397059,0.945419562447986,-1.50379521432319));
#20994=CARTESIAN_POINT('Ctrl Pts',(90.8185877636448,0.934885400320164,-1.51036667927128));
#20995=CARTESIAN_POINT('Ctrl Pts',(90.8172114317362,0.917693747247497,-1.52084245919051));
#20996=CARTESIAN_POINT('Ctrl Pts',(90.8166865660631,0.9110784080089,-1.5248146574681));
#20997=CARTESIAN_POINT('Ctrl Pts',(90.8156532864398,0.897933082823401,-1.53259171090727));
#20998=CARTESIAN_POINT('Ctrl Pts',(90.8151447789665,0.891404313136447,-1.53639823241275));
#20999=CARTESIAN_POINT('Ctrl Pts',(90.8138604974275,0.874769983140016,-1.54595495362762));
#21000=CARTESIAN_POINT('Ctrl Pts',(90.8130882675209,0.864631687947918,-1.55164793176589));
#21001=CARTESIAN_POINT('Ctrl Pts',(90.8098865072588,0.822065033990778,-1.57500369930661));
#21002=CARTESIAN_POINT('Ctrl Pts',(90.8075075202307,0.789143504051327,-1.59175391999361));
#21003=CARTESIAN_POINT('Ctrl Pts',(90.8006704748321,0.691624943064671,-1.63760048905792));
#21004=CARTESIAN_POINT('Ctrl Pts',(90.7963129016204,0.62577931754347,-1.6638756026224));
#21005=CARTESIAN_POINT('Ctrl Pts',(90.7845341755375,0.443767916978714,-1.72416683095149));
#21006=CARTESIAN_POINT('Ctrl Pts',(90.7771354360945,0.32543061719361,-1.75036346409506));
#21007=CARTESIAN_POINT('Ctrl Pts',(90.7677757053837,0.181156153830908,-1.76715592626368));
#21008=CARTESIAN_POINT('Ctrl Pts',(90.7661920588337,0.156902094767095,-1.7694742893946));
#21009=CARTESIAN_POINT('Ctrl Pts',(90.7635647029708,0.116984098866945,-1.77246277443643));
#21010=CARTESIAN_POINT('Ctrl Pts',(90.7625300976698,0.101344908574899,-1.77342571015882));
#21011=CARTESIAN_POINT('Ctrl Pts',(90.7606425602253,0.0729715253140104,
-1.7747961839436));
#21012=CARTESIAN_POINT('Ctrl Pts',(90.7597918812898,0.0602416677140853,
-1.77527385633855));
#21013=CARTESIAN_POINT('Ctrl Pts',(90.7579410476485,0.0326767663451601,
-1.77601137833165));
#21014=CARTESIAN_POINT('Ctrl Pts',(90.7569394271945,0.0178414967196386,
-1.77622235228174));
#21015=CARTESIAN_POINT('Ctrl Pts',(90.7541031093799,-0.023925986262745,
-1.7762930298592));
#21016=CARTESIAN_POINT('Ctrl Pts',(90.7522553276262,-0.050853866988934,
-1.77572608435241));
#21017=CARTESIAN_POINT('Ctrl Pts',(90.7440044955107,-0.169795627824018,
-1.77051428714231));
#21018=CARTESIAN_POINT('Ctrl Pts',(90.7374058369908,-0.261367302710889,
-1.75932771822355));
#21019=CARTESIAN_POINT('Ctrl Pts',(90.7232913756903,-0.45145846185995,-1.72093523936765));
#21020=CARTESIAN_POINT('Ctrl Pts',(90.7157767048709,-0.549352705534145,
-1.6922308459127));
#21021=CARTESIAN_POINT('Ctrl Pts',(90.7059473023638,-0.677331225236316,
-1.64242097110127));
#21022=CARTESIAN_POINT('Ctrl Pts',(90.7034374861994,-0.710022118810011,
-1.62855556314141));
#21023=CARTESIAN_POINT('Ctrl Pts',(90.7001591121276,-0.75299511728136,-1.60878885427543));
#21024=CARTESIAN_POINT('Ctrl Pts',(90.6993470035675,-0.763663369219857,
-1.60375231933771));
#21025=CARTESIAN_POINT('Ctrl Pts',(90.6980746875968,-0.780425713776407,
-1.59563353648172));
#21026=CARTESIAN_POINT('Ctrl Pts',(90.6976103696032,-0.786553340724527,
-1.59262190229232));
#21027=CARTESIAN_POINT('Ctrl Pts',(90.696645936336,-0.799305899429894,-1.58626266213039));
#21028=CARTESIAN_POINT('Ctrl Pts',(90.6961462786212,-0.805927425707033,
-1.58290875947911));
#21029=CARTESIAN_POINT('Ctrl Pts',(90.6948994178961,-0.822481932274537,
-1.57439284733317));
#21030=CARTESIAN_POINT('Ctrl Pts',(90.6941554400321,-0.832387727467028,
-1.56917814606081));
#21031=CARTESIAN_POINT('Ctrl Pts',(90.6911972819851,-0.871851764224807,
-1.54792424135628));
#21032=CARTESIAN_POINT('Ctrl Pts',(90.6890252509883,-0.901003137123161,
-1.5311396566469));
#21033=CARTESIAN_POINT('Ctrl Pts',(90.6830331206487,-0.981246263259831,
-1.48185175560645));
#21034=CARTESIAN_POINT('Ctrl Pts',(90.6792878284999,-1.0311802942413,-1.44754864361974));
#21035=CARTESIAN_POINT('Ctrl Pts',(90.6669623961319,-1.19040909168765,-1.32573450536113));
#21036=CARTESIAN_POINT('Ctrl Pts',(90.6584842110468,-1.29110182760245,-1.22788345258922));
#21037=CARTESIAN_POINT('Ctrl Pts',(90.6478323179766,-1.39509742716565,-1.09972651356004));
#21038=CARTESIAN_POINT('Ctrl Pts',(90.6461959404316,-1.41051145869358,-1.07988543743793));
#21039=CARTESIAN_POINT('Ctrl Pts',(90.6435865104896,-1.4341714663286,-1.04805895605372));
#21040=CARTESIAN_POINT('Ctrl Pts',(90.6426245948387,-1.44270025403382,-1.036287279633));
#21041=CARTESIAN_POINT('Ctrl Pts',(90.6408148979829,-1.45838001792699,-1.01407684773768));
#21042=CARTESIAN_POINT('Ctrl Pts',(90.6399685370063,-1.46556583929526,-1.00366373158723));
#21043=CARTESIAN_POINT('Ctrl Pts',(90.6380569717653,-1.48146192454421,-0.980093659727605));
#21044=CARTESIAN_POINT('Ctrl Pts',(90.636989467301,-1.49010924724986,-0.966895764150478));
#21045=CARTESIAN_POINT('Ctrl Pts',(90.6337259950201,-1.51584331029082,-0.926454120866957));
#21046=CARTESIAN_POINT('Ctrl Pts',(90.631509579253,-1.53236624868443,-0.898861293022755));
#21047=CARTESIAN_POINT('Ctrl Pts',(90.6234173790807,-1.58925703770875,-0.7977236724954));
#21048=CARTESIAN_POINT('Ctrl Pts',(90.6173947836576,-1.6251475718814,-0.721798491952967));
#21049=CARTESIAN_POINT('Ctrl Pts',(90.6038138162076,-1.69273239929099,-0.547957992802273));
#21050=CARTESIAN_POINT('Ctrl Pts',(90.5962347370852,-1.72156485035034,-0.449239680180405));
#21051=CARTESIAN_POINT('Ctrl Pts',(90.5864322471817,-1.74845905521874,-0.314861304597428));
#21052=CARTESIAN_POINT('Ctrl Pts',(90.5840022961059,-1.75422770488908,-0.280948810899604));
#21053=CARTESIAN_POINT('Ctrl Pts',(90.5808126636568,-1.76062515771961,-0.235368686768145));
#21054=CARTESIAN_POINT('Ctrl Pts',(90.5800119666206,-1.76212879212487,-0.223833650245843));
#21055=CARTESIAN_POINT('Ctrl Pts',(90.5787543717479,-1.76432901311362,-0.205555653267928));
#21056=CARTESIAN_POINT('Ctrl Pts',(90.5782934819438,-1.76510047699653,-0.198822290355401));
#21057=CARTESIAN_POINT('Ctrl Pts',(90.577326440946,-1.76664567259632,-0.184617304969676));
#21058=CARTESIAN_POINT('Ctrl Pts',(90.576820805837,-1.76741059025658,-0.177144834056858));
#21059=CARTESIAN_POINT('Ctrl Pts',(90.5755527948373,-1.76921903364286,-0.158298807376265));
#21060=CARTESIAN_POINT('Ctrl Pts',(90.5747937872704,-1.77020032877952,-0.146919414814571));
#21061=CARTESIAN_POINT('Ctrl Pts',(90.5717285552652,-1.77374464984017,-0.100603456763478));
#21062=CARTESIAN_POINT('Ctrl Pts',(90.5694676523215,-1.775383882622,-0.0656017469455326));
#21063=CARTESIAN_POINT('Ctrl Pts',(90.5631338560187,-1.7770984862331,0.0340034011332461));
#21064=CARTESIAN_POINT('Ctrl Pts',(90.559144938162,-1.77468737191219,0.0985958262223297));
#21065=CARTESIAN_POINT('Ctrl Pts',(90.54703751644,-1.75662537261308,0.294691684681125));
#21066=CARTESIAN_POINT('Ctrl Pts',(90.5389818428074,-1.72980243366558,0.42468262781185));
#21067=CARTESIAN_POINT('Ctrl Pts',(90.5287631777443,-1.68070754224882,0.575297587422005));
#21068=CARTESIAN_POINT('Ctrl Pts',(90.527063910504,-1.67207396965095,0.599928065069647));
#21069=CARTESIAN_POINT('Ctrl Pts',(90.5243698980803,-1.65768119532713,0.638261435568397));
#21070=CARTESIAN_POINT('Ctrl Pts',(90.5233872202813,-1.65228710791401,0.652098072452742));
#21071=CARTESIAN_POINT('Ctrl Pts',(90.5215474468001,-1.64192614026216,0.677721303937154));
#21072=CARTESIAN_POINT('Ctrl Pts',(90.5206919085464,-1.6370041927749,0.689525107620895));
#21073=CARTESIAN_POINT('Ctrl Pts',(90.51877100643,-1.62572530325261,0.715772524957874));
#21074=CARTESIAN_POINT('Ctrl Pts',(90.5177034627051,-1.61930254436453,0.730186490586994));
#21075=CARTESIAN_POINT('Ctrl Pts',(90.5144793100564,-1.59944980931749,0.773189502109483));
#21076=CARTESIAN_POINT('Ctrl Pts',(90.5123034561485,-1.58544908565549,0.801506503654535));
#21077=CARTESIAN_POINT('Ctrl Pts',(90.504084304135,-1.53036654106553,0.905816518903952));
#21078=CARTESIAN_POINT('Ctrl Pts',(90.4978844002723,-1.48451873790832,0.97914549612045));
#21079=CARTESIAN_POINT('Ctrl Pts',(90.4839080985347,-1.37111392453091,1.13414396369614));
#21080=CARTESIAN_POINT('Ctrl Pts',(90.4761128415445,-1.30121136469294,1.21370765009496));
#21081=CARTESIAN_POINT('Ctrl Pts',(90.46643890602,-1.20277415857796,1.30740595006728));
#21082=CARTESIAN_POINT('Ctrl Pts',(90.4643140275816,-1.18037180431038,1.32766661985536));
#21083=CARTESIAN_POINT('Ctrl Pts',(90.4614517724146,-1.14898265714858,1.35463201005526));
#21084=CARTESIAN_POINT('Ctrl Pts',(90.4606835312438,-1.14043425739005,1.36183653565372));
#21085=CARTESIAN_POINT('Ctrl Pts',(90.4594130047932,-1.12608091232583,1.37370348211296));
#21086=CARTESIAN_POINT('Ctrl Pts',(90.4589076455416,-1.1203137655118,1.37841087964511));
#21087=CARTESIAN_POINT('Ctrl Pts',(90.4578622236763,-1.10825967514635,1.38812432150205));
#21088=CARTESIAN_POINT('Ctrl Pts',(90.4573225672702,-1.10196813748527,1.39312414010998));
#21089=CARTESIAN_POINT('Ctrl Pts',(90.4558914620666,-1.08510617249149,1.40633845789726));
#21090=CARTESIAN_POINT('Ctrl Pts',(90.4550050455433,-1.07447622010225,1.41447663192102));
#21091=CARTESIAN_POINT('Ctrl Pts',(90.4503376224201,-1.01758251620421,1.45702229459449));
#21092=CARTESIAN_POINT('Ctrl Pts',(90.4466795344339,-0.969751438643358,
1.48928562257418));
#21093=CARTESIAN_POINT('Ctrl Pts',(90.4385254596719,-0.858162831344932,
1.55689474843891));
#21094=CARTESIAN_POINT('Ctrl Pts',(90.4340679726641,-0.793632347699398,
1.59075863465574));
#21095=CARTESIAN_POINT('Ctrl Pts',(90.4235431140112,-0.638078331995184,
1.66056104955992));
#21096=CARTESIAN_POINT('Ctrl Pts',(90.4174577494542,-0.545815868431496,
1.69312986752891));
#21097=CARTESIAN_POINT('Ctrl Pts',(90.4096559488324,-0.429481479981975,
1.72369399568845));
#21098=CARTESIAN_POINT('Ctrl Pts',(90.4081773400052,-0.407505491656879,
1.72902126432773));
#21099=CARTESIAN_POINT('Ctrl Pts',(90.4057593236647,-0.371730440535109,
1.73697369732101));
#21100=CARTESIAN_POINT('Ctrl Pts',(90.4048280957307,-0.357991015325491,
1.73985733889243));
#21101=CARTESIAN_POINT('Ctrl Pts',(90.4030199872131,-0.33139827621741,1.74511032154339));
#21102=CARTESIAN_POINT('Ctrl Pts',(90.4021438514935,-0.318550121125323,
1.74750126081862));
#21103=CARTESIAN_POINT('Ctrl Pts',(90.4000798891294,-0.288379170163522,
1.75277205160587));
#21104=CARTESIAN_POINT('Ctrl Pts',(90.3988885488663,-0.27103799993061,1.75553717561614));
#21105=CARTESIAN_POINT('Ctrl Pts',(90.3948476544138,-0.212487310191983,
1.76398515304366));
#21106=CARTESIAN_POINT('Ctrl Pts',(90.3919617861875,-0.171122654339681,
1.76847703413931));
#21107=CARTESIAN_POINT('Ctrl Pts',(90.3846678953406,-0.0677439472668281,
1.77604240285535));
#21108=CARTESIAN_POINT('Ctrl Pts',(90.3802134746023,-0.0056573794241821,
1.77732455496254));
#21109=CARTESIAN_POINT('Ctrl Pts',(90.3670967695023,0.174895057219392,1.77159238430677));
#21110=CARTESIAN_POINT('Ctrl Pts',(90.3583119772578,0.292750020355315,1.75596859022942));
#21111=CARTESIAN_POINT('Ctrl Pts',(90.3498698986825,0.408169026503127,1.72871689651704));
#21112=CARTESIAN_POINT('',(90.3498698986825,-1.48890580190326,0.968619417293912));
#21113=CARTESIAN_POINT('Origin',(90.3498698986825,0.,0.));
#21114=CARTESIAN_POINT('Ctrl Pts',(90.3498698986825,-1.48890580190324,0.968619417293899));
#21115=CARTESIAN_POINT('Ctrl Pts',(90.3538563142452,-1.52125431666485,0.918895149483884));
#21116=CARTESIAN_POINT('Ctrl Pts',(90.3577455404558,-1.55108810095714,0.867478027813688));
#21117=CARTESIAN_POINT('Ctrl Pts',(90.3615871323241,-1.57825856532581,0.814657819541863));
#21118=CARTESIAN_POINT('Ctrl Pts',(90.3619810187035,-1.58104440937268,0.80924205407051));
#21119=CARTESIAN_POINT('Ctrl Pts',(90.3623744043114,-1.58380226099585,0.803811582878728));
#21120=CARTESIAN_POINT('Ctrl Pts',(90.3627673425631,-1.58653196531297,0.79836674871169));
#21121=CARTESIAN_POINT('Ctrl Pts',(90.3670119182073,-1.61601862488144,0.739550865070549));
#21122=CARTESIAN_POINT('Ctrl Pts',(90.3712050420279,-1.64222035080938,0.679053296202822));
#21123=CARTESIAN_POINT('Ctrl Pts',(90.3754073490847,-1.6649903892128,0.617281304883328));
#21124=CARTESIAN_POINT('Ctrl Pts',(90.379587284972,-1.68763921029854,0.555838159521998));
#21125=CARTESIAN_POINT('Ctrl Pts',(90.3837767749571,-1.70689329459749,0.493134426296299));
#21126=CARTESIAN_POINT('Ctrl Pts',(90.3880198339045,-1.72265438865196,0.429574094169994));
#21127=CARTESIAN_POINT('Ctrl Pts',(90.3922629594753,-1.73841573018284,0.366012764036609));
#21128=CARTESIAN_POINT('Ctrl Pts',(90.3965599313326,-1.75068430678455,0.301594930371655));
#21129=CARTESIAN_POINT('Ctrl Pts',(90.4009335405249,-1.75940186175885,0.236724745270866));
#21130=CARTESIAN_POINT('Ctrl Pts',(90.405308475957,-1.7681220602179,0.171834889133232));
#21131=CARTESIAN_POINT('Ctrl Pts',(90.4097602207429,-1.77328927467888,0.10649243312025));
#21132=CARTESIAN_POINT('Ctrl Pts',(90.4142873758366,-1.77488127340981,0.0411009767190024));
#21133=CARTESIAN_POINT('Ctrl Pts',(90.4188550969619,-1.77648753740658,-0.024876426449256));
#21134=CARTESIAN_POINT('Ctrl Pts',(90.4234996199107,-1.77445421991782,-0.0909037515290607));
#21135=CARTESIAN_POINT('Ctrl Pts',(90.4281935981655,-1.76879385216752,-0.156567278160123));
#21136=CARTESIAN_POINT('Ctrl Pts',(90.4328560318523,-1.76317152333553,-0.221789531425848));
#21137=CARTESIAN_POINT('Ctrl Pts',(90.4375670778683,-1.75397062604308,-0.286652943004453));
#21138=CARTESIAN_POINT('Ctrl Pts',(90.4422756562143,-1.7412388162352,-0.350751928860527));
#21139=CARTESIAN_POINT('Ctrl Pts',(90.4470320197127,-1.72837779726297,-0.415501425250696));
#21140=CARTESIAN_POINT('Ctrl Pts',(90.4517855276462,-1.71191336093139,-0.479470963433884));
#21141=CARTESIAN_POINT('Ctrl Pts',(90.4564623747301,-1.69193526026765,-0.542241124442562));
#21142=CARTESIAN_POINT('Ctrl Pts',(90.4606543295379,-1.67402847528455,-0.598503318504739));
#21143=CARTESIAN_POINT('Ctrl Pts',(90.4647841420072,-1.65329854864641,-0.653802855979749));
#21144=CARTESIAN_POINT('Ctrl Pts',(90.4687890441026,-1.6298447879185,-0.707834103636427));
#21145=CARTESIAN_POINT('Ctrl Pts',(90.4692522995958,-1.6271318418251,-0.714084012295091));
#21146=CARTESIAN_POINT('Ctrl Pts',(90.4697138837835,-1.62438246579518,-0.720317006591094));
#21147=CARTESIAN_POINT('Ctrl Pts',(90.4701736995197,-1.62159682426134,-0.726532657354804));
#21148=CARTESIAN_POINT('Ctrl Pts',(90.4701754501884,-1.62158621841431,-0.726556322367136));
#21149=CARTESIAN_POINT('Ctrl Pts',(90.4701772008335,-1.62157561202607,-0.726579987165501));
#21150=CARTESIAN_POINT('Ctrl Pts',(90.470178951455,-1.62156500509664,-0.726603651749862));
#21151=CARTESIAN_POINT('Ctrl Pts',(90.47399760591,-1.59842796628609,-0.778223530068028));
#21152=CARTESIAN_POINT('Ctrl Pts',(90.4777041248918,-1.57271198408437,-0.828827245037696));
#21153=CARTESIAN_POINT('Ctrl Pts',(90.4813509415062,-1.54454993674521,-0.878148106426725));
#21154=CARTESIAN_POINT('Ctrl Pts',(90.4817603601505,-1.54138825672098,-0.883685231634755));
#21155=CARTESIAN_POINT('Ctrl Pts',(90.4821690263079,-1.5381957948568,-0.889206163508004));
#21156=CARTESIAN_POINT('Ctrl Pts',(90.4825770141721,-1.53497277616297,-0.894710507219073));
#21157=CARTESIAN_POINT('Ctrl Pts',(90.486565021165,-1.50346835601027,-0.94851446351322));
#21158=CARTESIAN_POINT('Ctrl Pts',(90.4904889952222,-1.46903946690765,-1.00073583159466));
#21159=CARTESIAN_POINT('Ctrl Pts',(90.4944116230711,-1.43190267812393,-1.05105650382837));
#21160=CARTESIAN_POINT('Ctrl Pts',(90.4946259244998,-1.4298738170642,-1.05380562823408));
#21161=CARTESIAN_POINT('Ctrl Pts',(90.4948402219106,-1.42783688463797,-1.05654907261513));
#21162=CARTESIAN_POINT('Ctrl Pts',(90.495054525525,-1.42579191997013,-1.05928678275577));
#21163=CARTESIAN_POINT('Ctrl Pts',(90.4990196573749,-1.38795515944602,-1.10994099923413));
#21164=CARTESIAN_POINT('Ctrl Pts',(90.5029872835318,-1.34736523212034,-1.15863524651694));
#21165=CARTESIAN_POINT('Ctrl Pts',(90.5070063827528,-1.30427777250265,-1.20507464471594));
#21166=CARTESIAN_POINT('Ctrl Pts',(90.5110226047008,-1.26122115919562,-1.25148079695157));
#21167=CARTESIAN_POINT('Ctrl Pts',(90.5150904846149,-1.21567087598052,-1.29563546976753));
#21168=CARTESIAN_POINT('Ctrl Pts',(90.519238130043,-1.16790637143662,-1.33727572254209));
#21169=CARTESIAN_POINT('Ctrl Pts',(90.5233843674953,-1.12015808121726,-1.37890183995444));
#21170=CARTESIAN_POINT('Ctrl Pts',(90.5276104382176,-1.07019723849451,-1.41801532460637));
#21171=CARTESIAN_POINT('Ctrl Pts',(90.5319208490151,-1.01832400466784,-1.45438312205025));
#21172=CARTESIAN_POINT('Ctrl Pts',(90.5362314191256,-0.966448853603774,
-1.4907522636498));
#21173=CARTESIAN_POINT('Ctrl Pts',(90.5406263480194,-0.912661235175542,
-1.52437552719678));
#21174=CARTESIAN_POINT('Ctrl Pts',(90.5450855649199,-0.857280619042244,
-1.55504875905309));
#21175=CARTESIAN_POINT('Ctrl Pts',(90.5495495604224,-0.80184065573558,-1.58575486106751));
#21176=CARTESIAN_POINT('Ctrl Pts',(90.554077878698,-0.74480423322187,-1.61350452338537));
#21177=CARTESIAN_POINT('Ctrl Pts',(90.5586264001637,-0.686511008695593,
-1.63812241542801));
#21178=CARTESIAN_POINT('Ctrl Pts',(90.5631778158279,-0.628180692520079,
-1.66275597169618));
#21179=CARTESIAN_POINT('Ctrl Pts',(90.5677491887434,-0.56859182097684,-1.68425353719366));
#21180=CARTESIAN_POINT('Ctrl Pts',(90.5722750656712,-0.508105382050814,
-1.70247122901301));
#21181=CARTESIAN_POINT('Ctrl Pts',(90.5765173364677,-0.451409219619926,
-1.71954734116053));
#21182=CARTESIAN_POINT('Ctrl Pts',(90.5807191840371,-0.393923833804837,
-1.73374174739534));
#21183=CARTESIAN_POINT('Ctrl Pts',(90.5848140042572,-0.335967087298439,
-1.74496526177759));
#21184=CARTESIAN_POINT('Ctrl Pts',(90.5850952976667,-0.331985752356128,
-1.74573626037015));
#21185=CARTESIAN_POINT('Ctrl Pts',(90.5853760860147,-0.328002178447056,
-1.74649325361629));
#21186=CARTESIAN_POINT('Ctrl Pts',(90.5856563477101,-0.324016461984582,
-1.74723621877522));
#21187=CARTESIAN_POINT('Ctrl Pts',(90.586974240284,-0.305274171430572,-1.7507299115683));
#21188=CARTESIAN_POINT('Ctrl Pts',(90.5882804122919,-0.286485050445651,
-1.75391334329275));
#21189=CARTESIAN_POINT('Ctrl Pts',(90.5895724730613,-0.26766022811415,-1.75678435040296));
#21190=CARTESIAN_POINT('Ctrl Pts',(90.5895746269833,-0.267628846309676,
-1.75678913649773));
#21191=CARTESIAN_POINT('Ctrl Pts',(90.5895767808694,-0.267597464341494,
-1.75679392173609));
#21192=CARTESIAN_POINT('Ctrl Pts',(90.5895789347197,-0.267566082209624,
-1.75679870611799));
#21193=CARTESIAN_POINT('Ctrl Pts',(90.5934312878049,-0.211436344065201,
-1.76535599930008));
#21194=CARTESIAN_POINT('Ctrl Pts',(90.5971689910853,-0.154779224758392,
-1.7711712273231));
#21195=CARTESIAN_POINT('Ctrl Pts',(90.6008427914221,-0.0978911430855949,
-1.77421564503471));
#21196=CARTESIAN_POINT('Ctrl Pts',(90.6012855002881,-0.0910358826428607,
-1.77458251056605));
#21197=CARTESIAN_POINT('Ctrl Pts',(90.6017272812006,-0.084177321001716,
-1.77490917335082));
#21198=CARTESIAN_POINT('Ctrl Pts',(90.6021682229604,-0.0773160193275386,
-1.77519561121616));
#21199=CARTESIAN_POINT('Ctrl Pts',(90.6063891314751,-0.0116363099084832,
-1.77793753347171));
#21200=CARTESIAN_POINT('Ctrl Pts',(90.6105340022366,0.0543000403042987,
-1.77699014460809));
#21201=CARTESIAN_POINT('Ctrl Pts',(90.6146743800401,0.120045333876444,-1.77237148682125));
#21202=CARTESIAN_POINT('Ctrl Pts',(90.6186870951359,0.183763464084872,-1.76789523883056));
#21203=CARTESIAN_POINT('Ctrl Pts',(90.6226960186818,0.247302095079509,-1.75997141185029));
#21204=CARTESIAN_POINT('Ctrl Pts',(90.6267510949758,0.310267424014638,-1.7486612585104));
#21205=CARTESIAN_POINT('Ctrl Pts',(90.6308036507985,0.37319361624946,-1.73735813510412));
#21206=CARTESIAN_POINT('Ctrl Pts',(90.6349025817534,0.435547204357498,-1.7226732392878));
#21207=CARTESIAN_POINT('Ctrl Pts',(90.6390770766321,0.496949467663568,-1.70470523642112));
#21208=CARTESIAN_POINT('Ctrl Pts',(90.6432504727539,0.558335569455983,-1.68674196286094));
#21209=CARTESIAN_POINT('Ctrl Pts',(90.6474995272466,0.6187708514289,-1.66549750550593));
#21210=CARTESIAN_POINT('Ctrl Pts',(90.6518296869147,0.677891277099393,-1.64110394788305));
#21211=CARTESIAN_POINT('Ctrl Pts',(90.6561602585123,0.737017326914143,-1.61670806969355));
#21212=CARTESIAN_POINT('Ctrl Pts',(90.6605719693885,0.794828270312418,-1.5891625530848));
#21213=CARTESIAN_POINT('Ctrl Pts',(90.66504540428,0.850974313885249,-1.55863110702535));
#21214=CARTESIAN_POINT('Ctrl Pts',(90.6695236925955,0.907181272741975,-1.52806653607256));
#21215=CARTESIAN_POINT('Ctrl Pts',(90.674063737033,0.961719693086612,-1.49450945947954));
#21216=CARTESIAN_POINT('Ctrl Pts',(90.6786217336073,1.01425317371748,-1.4581559940994));
#21217=CARTESIAN_POINT('Ctrl Pts',(90.6831827264511,1.06682118804405,-1.42177863120674));
#21218=CARTESIAN_POINT('Ctrl Pts',(90.6877614187742,1.11738152335539,-1.38260092592077));
#21219=CARTESIAN_POINT('Ctrl Pts',(90.6922923521835,1.16561251953689,-1.34085402094085));
#21220=CARTESIAN_POINT('Ctrl Pts',(90.6965307994336,1.21073005154868,-1.30180201142529));
#21221=CARTESIAN_POINT('Ctrl Pts',(90.7007269946079,1.25380961442412,-1.26050123889405));
#21222=CARTESIAN_POINT('Ctrl Pts',(90.7048145774088,1.29460112222741,-1.21717422755039));
#21223=CARTESIAN_POINT('Ctrl Pts',(90.7051038995783,1.29748837567578,-1.214107509264));
#21224=CARTESIAN_POINT('Ctrl Pts',(90.7053926776092,1.30036418725321,-1.21103063464629));
#21225=CARTESIAN_POINT('Ctrl Pts',(90.7056808879696,1.30322847787149,-1.20794368006088));
#21226=CARTESIAN_POINT('Ctrl Pts',(90.706642560046,1.31278576200889,-1.19764343262661));
#21227=CARTESIAN_POINT('Ctrl Pts',(90.7075978710689,1.32221459126303,-1.18723119764786));
#21228=CARTESIAN_POINT('Ctrl Pts',(90.7085458919079,1.33151184766431,-1.1767102021235));
#21229=CARTESIAN_POINT('Ctrl Pts',(90.7085477520551,1.33153009015947,-1.17668955848396));
#21230=CARTESIAN_POINT('Ctrl Pts',(90.7085496121766,1.33154833217906,-1.17666891439259));
#21231=CARTESIAN_POINT('Ctrl Pts',(90.7085514722723,1.33156657372303,-1.17664826984943));
#21232=CARTESIAN_POINT('Ctrl Pts',(90.7124095359009,1.36940174310797,-1.13382898936784));
#21233=CARTESIAN_POINT('Ctrl Pts',(90.7161568944749,1.40519106883275,-1.08906167835935));
#21234=CARTESIAN_POINT('Ctrl Pts',(90.7198447048519,1.43874779482561,-1.04258403106708));
#21235=CARTESIAN_POINT('Ctrl Pts',(90.7202667374043,1.44258802229817,-1.03726513499749));
#21236=CARTESIAN_POINT('Ctrl Pts',(90.7206879900847,1.44639900936124,-1.03192389566102));
#21237=CARTESIAN_POINT('Ctrl Pts',(90.721108539565,1.45018047627668,-1.02656071269748));
#21238=CARTESIAN_POINT('Ctrl Pts',(90.7251999964893,1.48696974774802,-0.974383185190741));
#21239=CARTESIAN_POINT('Ctrl Pts',(90.729225622378,1.52096537489848,-0.920122745683341));
#21240=CARTESIAN_POINT('Ctrl Pts',(90.7332498753217,1.55195968493651,-0.864131848584758));
#21241=CARTESIAN_POINT('Ctrl Pts',(90.7372699500544,1.58292181489895,-0.808199084456343));
#21242=CARTESIAN_POINT('Ctrl Pts',(90.7412891299274,1.61088923626005,-0.750539827506467));
#21243=CARTESIAN_POINT('Ctrl Pts',(90.7453565652005,1.63569909853021,-0.69151804308843));
#21244=CARTESIAN_POINT('Ctrl Pts',(90.7494217935304,1.66049549925754,-0.632528283204455));
#21245=CARTESIAN_POINT('Ctrl Pts',(90.7535355012154,1.68213804425792,-0.572177673540597));
#21246=CARTESIAN_POINT('Ctrl Pts',(90.7577260849918,1.70050334020167,-0.510837996941952));
#21247=CARTESIAN_POINT('Ctrl Pts',(90.7619153268021,1.71886275495941,-0.449517963372648));
#21248=CARTESIAN_POINT('Ctrl Pts',(90.7661815269526,1.73394718308619,-0.387209598446523));
#21249=CARTESIAN_POINT('Ctrl Pts',(90.7705293740152,1.74566922202807,-0.324290519440164));
#21250=CARTESIAN_POINT('Ctrl Pts',(90.7748788694906,1.7573957051829,-0.261347585728403));
#21251=CARTESIAN_POINT('Ctrl Pts',(90.7793100912484,1.76575729635694,-0.19779350654627));
#21252=CARTESIAN_POINT('Ctrl Pts',(90.7838029196334,1.77070081358476,-0.134011531087324));
#21253=CARTESIAN_POINT('Ctrl Pts',(90.7858318981217,1.77293332487895,-0.105207346937488));
#21254=CARTESIAN_POINT('Ctrl Pts',(90.7878731037697,1.77446919335584,-0.0763567518078401));
#21255=CARTESIAN_POINT('Ctrl Pts',(90.7899230490922,1.77530581490221,-0.0474953858958098));
#21256=CARTESIAN_POINT('Origin',(88.3562164250559,0.,0.));
#21257=CARTESIAN_POINT('',(91.6892085959652,1.77561363837197,-0.0475422940912394));
#21258=CARTESIAN_POINT('',(91.5422141974348,1.77561363837144,-0.0475422941110715));
#21259=CARTESIAN_POINT('',(88.3562164250559,1.77561363837197,-0.0475422940912398));
#21260=CARTESIAN_POINT('Ctrl Pts',(91.6892085959652,1.77561363837197,-0.0475422940912359));
#21261=CARTESIAN_POINT('Ctrl Pts',(91.6826296493429,1.77317281232423,-0.138702472666949));
#21262=CARTESIAN_POINT('Ctrl Pts',(91.6759149193743,1.76371331345252,-0.229614208752581));
#21263=CARTESIAN_POINT('Ctrl Pts',(91.6643821335648,1.73522339018167,-0.385436676345231));
#21264=CARTESIAN_POINT('Ctrl Pts',(91.6595491631098,1.71943375700664,-0.450678526944558));
#21265=CARTESIAN_POINT('Ctrl Pts',(91.6539287316192,1.69602371461896,-0.527972385438873));
#21266=CARTESIAN_POINT('Ctrl Pts',(91.6529836089651,1.69190619307101,-0.541021943213308));
#21267=CARTESIAN_POINT('Ctrl Pts',(91.6514999167809,1.68514750048711,-0.561609942369776));
#21268=CARTESIAN_POINT('Ctrl Pts',(91.6509559672094,1.68260567713873,-0.569180083416648));
#21269=CARTESIAN_POINT('Ctrl Pts',(91.6499223610523,1.67765126990361,-0.583612182041431));
#21270=CARTESIAN_POINT('Ctrl Pts',(91.6494322470786,1.67524747915378,-0.590476797094879));
#21271=CARTESIAN_POINT('Ctrl Pts',(91.6483456422136,1.66979780691413,-0.605738499458421));
#21272=CARTESIAN_POINT('Ctrl Pts',(91.6477503827448,1.66673057207595,-0.614127880956124));
#21273=CARTESIAN_POINT('Ctrl Pts',(91.6456999947142,1.65588627874564,-0.643108992245147));
#21274=CARTESIAN_POINT('Ctrl Pts',(91.6442621190886,1.64778950971065,-0.663579974064104));
#21275=CARTESIAN_POINT('Ctrl Pts',(91.6345175979573,1.58969180114976,-0.802841416987966));
#21276=CARTESIAN_POINT('Ctrl Pts',(91.6267615875747,1.52726583677266,-0.916046674103866));
#21277=CARTESIAN_POINT('Ctrl Pts',(91.6150501003413,1.4180051541739,-1.07147360270502));
#21278=CARTESIAN_POINT('Ctrl Pts',(91.611254650614,1.38032936482806,-1.11959114832423));
#21279=CARTESIAN_POINT('Ctrl Pts',(91.6047754119644,1.31335358689614,-1.19659788256551));
#21280=CARTESIAN_POINT('Ctrl Pts',(91.6021389272148,1.28539395364529,-1.22658310545357));
#21281=CARTESIAN_POINT('Ctrl Pts',(91.5983254879301,1.24417155307738,-1.26783344795948));
#21282=CARTESIAN_POINT('Ctrl Pts',(91.5971845319235,1.23174078880252,-1.27991370775004));
#21283=CARTESIAN_POINT('Ctrl Pts',(91.5951804954699,1.20975292009111,-1.30066459050129));
#21284=CARTESIAN_POINT('Ctrl Pts',(91.5943210110471,1.20027428264879,-1.30941671595651));
#21285=CARTESIAN_POINT('Ctrl Pts',(91.5925294649403,1.18042236884044,-1.32735035926103));
#21286=CARTESIAN_POINT('Ctrl Pts',(91.5915967881965,1.17003537112961,-1.33651530348929));
#21287=CARTESIAN_POINT('Ctrl Pts',(91.5891512859068,1.14267262055608,-1.36009532114593));
#21288=CARTESIAN_POINT('Ctrl Pts',(91.5876305633874,1.12553154597135,-1.37431388723694));
#21289=CARTESIAN_POINT('Ctrl Pts',(91.5800310116375,1.0392922044019,-1.44315400639718));
#21290=CARTESIAN_POINT('Ctrl Pts',(91.5737652270432,0.96647492198799,-1.49289778941215));
#21291=CARTESIAN_POINT('Ctrl Pts',(91.5598710806628,0.800631599885092,-1.58895757418608));
#21292=CARTESIAN_POINT('Ctrl Pts',(91.5522203315567,0.70661504025961,-1.63293965944108));
#21293=CARTESIAN_POINT('Ctrl Pts',(91.5425675423318,0.580764312996491,-1.67889841692755));
#21294=CARTESIAN_POINT('Ctrl Pts',(91.5403974382705,0.5519621084944,-1.68858672269114));
#21295=CARTESIAN_POINT('Ctrl Pts',(91.5367689921219,0.502736464015158,-1.70375066271102));
#21296=CARTESIAN_POINT('Ctrl Pts',(91.5352955943416,0.482438457589693,-1.70960916731568));
#21297=CARTESIAN_POINT('Ctrl Pts',(91.5331901230705,0.45291727772037,-1.71756201054307));
#21298=CARTESIAN_POINT('Ctrl Pts',(91.5325432470355,0.443775133870238,-1.719946790228));
#21299=CARTESIAN_POINT('Ctrl Pts',(91.5314112844725,0.427642142689588,-1.72401797105399));
#21300=CARTESIAN_POINT('Ctrl Pts',(91.5309245214273,0.420659502634534,-1.72573501902722));
#21301=CARTESIAN_POINT('Ctrl Pts',(91.5298580839211,0.405260617343389,-1.72942262057064));
#21302=CARTESIAN_POINT('Ctrl Pts',(91.5292794734823,0.396840210694156,-1.73137420089205));
#21303=CARTESIAN_POINT('Ctrl Pts',(91.5276171672606,0.372471492100008,-1.73683496566747));
#21304=CARTESIAN_POINT('Ctrl Pts',(91.52654190647,0.356488131968085,-1.74018590059446));
#21305=CARTESIAN_POINT('Ctrl Pts',(91.5177637555482,0.224422147541329,-1.76597766884389));
#21306=CARTESIAN_POINT('Ctrl Pts',(91.5105803185552,0.106394729830693,-1.7770004006878));
#21307=CARTESIAN_POINT('Ctrl Pts',(91.4967372440651,-0.119007806605712,
-1.775494608696));
#21308=CARTESIAN_POINT('Ctrl Pts',(91.4901175842461,-0.225852135552002,
-1.76508666694622));
#21309=CARTESIAN_POINT('Ctrl Pts',(91.4816202469844,-0.354956980557504,
-1.74059162395977));
#21310=CARTESIAN_POINT('Ctrl Pts',(91.4800361437933,-0.378716699610612,
-1.73557691505368));
#21311=CARTESIAN_POINT('Ctrl Pts',(91.4774963104821,-0.416267935295048,
-1.72684359669201));
#21312=CARTESIAN_POINT('Ctrl Pts',(91.4765507673244,-0.430130774113298,
-1.72344286197296));
#21313=CARTESIAN_POINT('Ctrl Pts',(91.4747482112428,-0.456327225807575,
-1.71668078219239));
#21314=CARTESIAN_POINT('Ctrl Pts',(91.4738923228931,-0.468668529293851,
-1.71335263149227));
#21315=CARTESIAN_POINT('Ctrl Pts',(91.4719257717743,-0.49679607990436,-1.70544067977924));
#21316=CARTESIAN_POINT('Ctrl Pts',(91.4708123545692,-0.512556564177838,
-1.70077041190923));
#21317=CARTESIAN_POINT('Ctrl Pts',(91.4672703569929,-0.562160449487276,
-1.68531932228674));
#21318=CARTESIAN_POINT('Ctrl Pts',(91.4648161591335,-0.595744656745387,
-1.67374238753223));
#21319=CARTESIAN_POINT('Ctrl Pts',(91.4521477258142,-0.765056985236665,
-1.60963672689961));
#21320=CARTESIAN_POINT('Ctrl Pts',(91.4414289212185,-0.89429196544866,-1.54158075779734));
#21321=CARTESIAN_POINT('Ctrl Pts',(91.4275552356117,-1.05079419334238,-1.43280508124705));
#21322=CARTESIAN_POINT('Ctrl Pts',(91.4242945118892,-1.08684280589143,-1.40565716048554));
#21323=CARTESIAN_POINT('Ctrl Pts',(91.4191120590128,-1.14342039327851,-1.35956978253387));
#21324=CARTESIAN_POINT('Ctrl Pts',(91.4171559705445,-1.16460467316928,-1.34146798437002));
#21325=CARTESIAN_POINT('Ctrl Pts',(91.4145056371625,-1.19317740923358,-1.31586550717301));
#21326=CARTESIAN_POINT('Ctrl Pts',(91.4137846105695,-1.20093707209892,-1.30878742559641));
#21327=CARTESIAN_POINT('Ctrl Pts',(91.4125691318587,-1.21400219346931,-1.29665585486836));
#21328=CARTESIAN_POINT('Ctrl Pts',(91.4120721361137,-1.21933992019365,-1.29163768097164));
#21329=CARTESIAN_POINT('Ctrl Pts',(91.4110341004383,-1.23048142611786,-1.28103255682529));
#21330=CARTESIAN_POINT('Ctrl Pts',(91.4104935745226,-1.23627845571372,-1.27543895896636));
#21331=CARTESIAN_POINT('Ctrl Pts',(91.4090208300729,-1.25205337650327,-1.26000901019667));
#21332=CARTESIAN_POINT('Ctrl Pts',(91.4080944865329,-1.26195350111415,-1.2500934984102));
#21333=CARTESIAN_POINT('Ctrl Pts',(91.4026309890176,-1.32012687176673,-1.1904342405566));
#21334=CARTESIAN_POINT('Ctrl Pts',(91.3982768200263,-1.36557762100826,-1.13801083333082));
#21335=CARTESIAN_POINT('Ctrl Pts',(91.3841997336238,-1.50415736935112,-0.957873106752965));
#21336=CARTESIAN_POINT('Ctrl Pts',(91.3747253165413,-1.58332890279708,-0.820413322369242));
#21337=CARTESIAN_POINT('Ctrl Pts',(91.3628929591193,-1.65292408720351,-0.650807756524253));
#21338=CARTESIAN_POINT('Ctrl Pts',(91.3612390717011,-1.66205784374785,-0.627114337891258));
#21339=CARTESIAN_POINT('Ctrl Pts',(91.3586045528446,-1.67565453493951,-0.589457781037764));
#21340=CARTESIAN_POINT('Ctrl Pts',(91.357635254108,-1.6804580860561,-0.575620704525858));
#21341=CARTESIAN_POINT('Ctrl Pts',(91.3558131153594,-1.68911436805312,-0.549653223728241));
#21342=CARTESIAN_POINT('Ctrl Pts',(91.354961723422,-1.69300893208587,-0.537537678715284));
#21343=CARTESIAN_POINT('Ctrl Pts',(91.3530404756013,-1.70145982160554,-0.510244678218971));
#21344=CARTESIAN_POINT('Ctrl Pts',(91.3519683282945,-1.70594385148206,-0.495046162841493));
#21345=CARTESIAN_POINT('Ctrl Pts',(91.3486957218741,-1.71892738420683,-0.448766036527064));
#21346=CARTESIAN_POINT('Ctrl Pts',(91.3464748878821,-1.72678463025911,-0.4175127700728));
#21347=CARTESIAN_POINT('Ctrl Pts',(91.3383938041444,-1.75197228212532,-0.304396974724843));
#21348=CARTESIAN_POINT('Ctrl Pts',(91.3323886517178,-1.76436213727278,-0.221556748651658));
#21349=CARTESIAN_POINT('Ctrl Pts',(91.318851184071,-1.77882871158686,-0.036133311173877));
#21350=CARTESIAN_POINT('Ctrl Pts',(91.311298450084,-1.77795670261595,0.0663929387965299));
#21351=CARTESIAN_POINT('Ctrl Pts',(91.3014914549188,-1.76496809820928,0.202879161166147));
#21352=CARTESIAN_POINT('Ctrl Pts',(91.2990352327657,-1.76065970613732,0.237381793567552));
#21353=CARTESIAN_POINT('Ctrl Pts',(91.2958149134345,-1.75355007352704,0.283307716586331));
#21354=CARTESIAN_POINT('Ctrl Pts',(91.2950090952338,-1.75164464678338,0.294859581185639));
#21355=CARTESIAN_POINT('Ctrl Pts',(91.2937442532734,-1.74845044291918,0.313099798006016));
#21356=CARTESIAN_POINT('Ctrl Pts',(91.2932811970449,-1.74723721852877,0.319800783322098));
#21357=CARTESIAN_POINT('Ctrl Pts',(91.2923135512147,-1.74460887521808,0.333856289440616));
#21358=CARTESIAN_POINT('Ctrl Pts',(91.2918094606678,-1.74318572793642,0.341209130491232));
#21359=CARTESIAN_POINT('Ctrl Pts',(91.2905462942246,-1.73948440211319,0.35970462812763));
#21360=CARTESIAN_POINT('Ctrl Pts',(91.2897905591451,-1.73714558373789,0.370835061012365));
#21361=CARTESIAN_POINT('Ctrl Pts',(91.2867447660612,-1.72721964964845,0.415916485012722));
#21362=CARTESIAN_POINT('Ctrl Pts',(91.2844995358084,-1.71874231725382,0.449665945880171));
#21363=CARTESIAN_POINT('Ctrl Pts',(91.278220956436,-1.69188131136068,0.544694845038104));
#21364=CARTESIAN_POINT('Ctrl Pts',(91.2742702238187,-1.67117127087735,0.605262383363768));
#21365=CARTESIAN_POINT('Ctrl Pts',(91.2621814589209,-1.59759844301491,0.787619886974256));
#21366=CARTESIAN_POINT('Ctrl Pts',(91.2541097007993,-1.53433742922395,0.904693575425017));
#21367=CARTESIAN_POINT('Ctrl Pts',(91.243882587421,-1.44385212322838,1.03490399280535));
#21368=CARTESIAN_POINT('Ctrl Pts',(91.2421959797649,-1.42860517980615,1.05585148427319));
#21369=CARTESIAN_POINT('Ctrl Pts',(91.239520953229,-1.40396148493965,1.0881976182194));
#21370=CARTESIAN_POINT('Ctrl Pts',(91.2385444676047,-1.39487102002495,1.09982576933207));
#21371=CARTESIAN_POINT('Ctrl Pts',(91.236715766698,-1.37767954658768,1.12126039952323));
#21372=CARTESIAN_POINT('Ctrl Pts',(91.2358650921355,-1.36961602115249,1.13109582118615));
#21373=CARTESIAN_POINT('Ctrl Pts',(91.2339546066057,-1.3513638053314,1.15287745578858));
#21374=CARTESIAN_POINT('Ctrl Pts',(91.2328926199139,-1.34112104741554,1.16477674725793));
#21375=CARTESIAN_POINT('Ctrl Pts',(91.2296846384023,-1.30990088729699,1.20008826832793));
#21376=CARTESIAN_POINT('Ctrl Pts',(91.2275194431717,-1.28845935797696,1.22307990355935));
#21377=CARTESIAN_POINT('Ctrl Pts',(91.2181797254625,-1.19446346038582,1.31865543700269));
#21378=CARTESIAN_POINT('Ctrl Pts',(91.2107685365086,-1.11631182134713,1.38543759136332));
#21379=CARTESIAN_POINT('Ctrl Pts',(91.1952796022268,-0.943812264325387,
1.50872754439353));
#21380=CARTESIAN_POINT('Ctrl Pts',(91.1872235286457,-0.849081913317272,
1.56400256004418));
#21381=CARTESIAN_POINT('Ctrl Pts',(91.1783627629608,-0.734399698618942,
1.61740904038376));
#21382=CARTESIAN_POINT('Ctrl Pts',(91.177178509981,-0.718835737319015,1.62438608631868));
#21383=CARTESIAN_POINT('Ctrl Pts',(91.1754021991818,-0.695095143840516,
1.63462050084888));
#21384=CARTESIAN_POINT('Ctrl Pts',(91.1748011063388,-0.686991311147375,
1.63804285276274));
#21385=CARTESIAN_POINT('Ctrl Pts',(91.1737647254907,-0.672891017507956,
1.64387453737232));
#21386=CARTESIAN_POINT('Ctrl Pts',(91.1733278330976,-0.666906513771491,
1.64631148974407));
#21387=CARTESIAN_POINT('Ctrl Pts',(91.1722957781207,-0.652673817102096,
1.6520168455186));
#21388=CARTESIAN_POINT('Ctrl Pts',(91.1717023414018,-0.644414274879106,
1.65525617961491));
#21389=CARTESIAN_POINT('Ctrl Pts',(91.1699164828718,-0.619342021985435,
1.66487322258765));
#21390=CARTESIAN_POINT('Ctrl Pts',(91.1687347436265,-0.602455842786204,
1.67105787033356));
#21391=CARTESIAN_POINT('Ctrl Pts',(91.162771832699,-0.515928927016828,1.70126659921716));
#21392=CARTESIAN_POINT('Ctrl Pts',(91.1581801474869,-0.444928778811952,
1.72120058994853));
#21393=CARTESIAN_POINT('Ctrl Pts',(91.1451208640453,-0.237936003479186,
1.76564503671502));
#21394=CARTESIAN_POINT('Ctrl Pts',(91.1367793607157,-0.100077466102164,
1.77879111975311));
#21395=CARTESIAN_POINT('Ctrl Pts',(91.1259691324007,0.0684302052589961,
1.77519386610434));
#21396=CARTESIAN_POINT('Ctrl Pts',(91.1239903103789,0.0989267311219573,
1.77375569895112));
#21397=CARTESIAN_POINT('Ctrl Pts',(91.1209554170376,0.145052983691987,1.77038723796495));
#21398=CARTESIAN_POINT('Ctrl Pts',(91.1199172749827,0.160719955518372,1.76903375032678));
#21399=CARTESIAN_POINT('Ctrl Pts',(91.118027343948,0.189026222953417,1.76620922157189));
#21400=CARTESIAN_POINT('Ctrl Pts',(91.1171778697097,0.201671733886498,1.76481002507206));
#21401=CARTESIAN_POINT('Ctrl Pts',(91.1153343871106,0.228940385422187,1.76149591092199));
#21402=CARTESIAN_POINT('Ctrl Pts',(91.1143389689357,0.243556800376245,1.75953448570266));
#21403=CARTESIAN_POINT('Ctrl Pts',(91.1115342241407,0.284428972079078,1.75353069081313));
#21404=CARTESIAN_POINT('Ctrl Pts',(91.1097122344657,0.310619992418844,1.74908113338163));
#21405=CARTESIAN_POINT('Ctrl Pts',(91.1016762603998,0.424522154356266,1.72709153131278));
#21406=CARTESIAN_POINT('Ctrl Pts',(91.0952783024372,0.510925356109155,1.70353025359939));
#21407=CARTESIAN_POINT('Ctrl Pts',(91.0817416384733,0.686325602147335,1.64115209257749));
#21408=CARTESIAN_POINT('Ctrl Pts',(91.0746066882567,0.774673825118238,1.60134435540629));
#21409=CARTESIAN_POINT('Ctrl Pts',(91.0646031844759,0.896357649723831,1.53407820097511));
#21410=CARTESIAN_POINT('Ctrl Pts',(91.0615982965574,0.932634486120392,1.51229841788795));
#21411=CARTESIAN_POINT('Ctrl Pts',(91.0577948544236,0.978571838050334,1.48243622496298));
#21412=CARTESIAN_POINT('Ctrl Pts',(91.0569340592789,0.988970018650634,1.47551968058925));
#21413=CARTESIAN_POINT('Ctrl Pts',(91.0555518560824,1.00568255691507,1.46414697219685));
#21414=CARTESIAN_POINT('Ctrl Pts',(91.0550262076812,1.01204208440103,1.45975840009881));
#21415=CARTESIAN_POINT('Ctrl Pts',(91.0539952907533,1.02452598220697,1.45102273340401));
#21416=CARTESIAN_POINT('Ctrl Pts',(91.0534898984312,1.0306517618313,1.44667806040265));
#21417=CARTESIAN_POINT('Ctrl Pts',(91.0522175478289,1.04608218375293,1.43558636768372));
#21418=CARTESIAN_POINT('Ctrl Pts',(91.0514540410584,1.05534944315585,1.42878750151326));
#21419=CARTESIAN_POINT('Ctrl Pts',(91.0483264004739,1.09330815410136,1.40036849207165));
#21420=CARTESIAN_POINT('Ctrl Pts',(91.0460102521039,1.12140847692253,1.37796882078168));
#21421=CARTESIAN_POINT('Ctrl Pts',(91.0394399909226,1.20032608829171,1.31104664658149));
#21422=CARTESIAN_POINT('Ctrl Pts',(91.0352780207815,1.24931012110267,1.26445699732421));
#21423=CARTESIAN_POINT('Ctrl Pts',(91.0233391421653,1.38228677708623,1.12268919506221));
#21424=CARTESIAN_POINT('Ctrl Pts',(91.0156033691866,1.45888449288332,1.02117568175833));
#21425=CARTESIAN_POINT('Ctrl Pts',(91.0058771395955,1.53639852186612,0.891697557030682));
#21426=CARTESIAN_POINT('Ctrl Pts',(91.0043102430581,1.54835573172312,0.87076942415628));
#21427=CARTESIAN_POINT('Ctrl Pts',(91.0017061903901,1.56733104967099,0.835930567722899));
#21428=CARTESIAN_POINT('Ctrl Pts',(91.0006779203798,1.57459875766763,0.822158901826114));
#21429=CARTESIAN_POINT('Ctrl Pts',(90.9987991609346,1.58746449824674,0.796982983104844));
#21430=CARTESIAN_POINT('Ctrl Pts',(90.9979508752841,1.59312309023943,0.785610726416097));
#21431=CARTESIAN_POINT('Ctrl Pts',(90.9961021399136,1.60512728941075,0.760822373759666));
#21432=CARTESIAN_POINT('Ctrl Pts',(90.9951001924201,1.61142765484908,0.747385569476833));
#21433=CARTESIAN_POINT('Ctrl Pts',(90.992254068052,1.62874243819139,0.709221299652784));
#21434=CARTESIAN_POINT('Ctrl Pts',(90.9903965864751,1.63936060905985,0.684319687436978));
#21435=CARTESIAN_POINT('Ctrl Pts',(90.9820411650697,1.68409381653847,0.572388993700153));
#21436=CARTESIAN_POINT('Ctrl Pts',(90.9753411044094,1.71187199064594,0.483001801999001));
#21437=CARTESIAN_POINT('Ctrl Pts',(90.960916186721,1.75557419121274,0.289784547682405));
#21438=CARTESIAN_POINT('Ctrl Pts',(90.9531908183237,1.76959579491818,0.18587013192019));
#21439=CARTESIAN_POINT('Ctrl Pts',(90.9434531987421,1.77584482714027,0.0495235656792568));
#21440=CARTESIAN_POINT('Ctrl Pts',(90.9412089529301,1.7764472631034,0.0176876180614906));
#21441=CARTESIAN_POINT('Ctrl Pts',(90.938233924654,1.776104960991,-0.025281661185769));
#21442=CARTESIAN_POINT('Ctrl Pts',(90.9374681330973,1.7759116246033,-0.0364130790099715));
#21443=CARTESIAN_POINT('Ctrl Pts',(90.9367078804582,1.77561363837197,-0.047542294091302));
#21444=CARTESIAN_POINT('Ctrl Pts',(90.7897454441732,1.7756150039535,-0.0474912648304961));
#21445=CARTESIAN_POINT('Ctrl Pts',(90.7993156250187,1.77915527271836,0.0848731680678009));
#21446=CARTESIAN_POINT('Ctrl Pts',(90.8091563929607,1.76788427360103,0.217214520202615));
#21447=CARTESIAN_POINT('Ctrl Pts',(90.8206238752608,1.73636860213996,0.375395942414399));
#21448=CARTESIAN_POINT('Ctrl Pts',(90.8226534426878,1.73003555099807,0.403578069599024));
#21449=CARTESIAN_POINT('Ctrl Pts',(90.825382050939,1.72044236685113,0.441876063702402));
#21450=CARTESIAN_POINT('Ctrl Pts',(90.8261099787572,1.71777505501923,0.452134125762967));
#21451=CARTESIAN_POINT('Ctrl Pts',(90.8273303954271,1.71311693854743,0.469412017096595));
#21452=CARTESIAN_POINT('Ctrl Pts',(90.8278255381535,1.7111744367089,0.476444478862312));
#21453=CARTESIAN_POINT('Ctrl Pts',(90.8288487216917,1.70704946125473,0.491027458977852));
#21454=CARTESIAN_POINT('Ctrl Pts',(90.8293763637131,1.70486011660728,0.498575789102205));
#21455=CARTESIAN_POINT('Ctrl Pts',(90.8307983899849,1.69879298132516,0.518986450415898));
#21456=CARTESIAN_POINT('Ctrl Pts',(90.8316874196534,1.69481916958428,0.531820024657418));
#21457=CARTESIAN_POINT('Ctrl Pts',(90.8363417341777,1.67307994049936,0.599308072673576));
#21458=CARTESIAN_POINT('Ctrl Pts',(90.8399813234926,1.65281367335895,0.653127112136689));
#21459=CARTESIAN_POINT('Ctrl Pts',(90.849886729446,1.58965465691844,0.798970979677874));
#21460=CARTESIAN_POINT('Ctrl Pts',(90.8560216604907,1.54143569642201,0.888444572145996));
#21461=CARTESIAN_POINT('Ctrl Pts',(90.865518575516,1.45741769331623,1.01670462959569));
#21462=CARTESIAN_POINT('Ctrl Pts',(90.8687634326733,1.42710939633498,1.05882615364145));
#21463=CARTESIAN_POINT('Ctrl Pts',(90.8736813970622,1.37934539289045,1.1194240156371));
#21464=CARTESIAN_POINT('Ctrl Pts',(90.8753072946828,1.36326576138031,1.13895136306727));
#21465=CARTESIAN_POINT('Ctrl Pts',(90.8783051339677,1.33315573808991,1.17396600176898));
#21466=CARTESIAN_POINT('Ctrl Pts',(90.8796717508298,1.3192584060519,1.18956193326501));
#21467=CARTESIAN_POINT('Ctrl Pts',(90.8819015095843,1.29633349395425,1.21439291759901));
#21468=CARTESIAN_POINT('Ctrl Pts',(90.8827574814467,1.28747432545772,1.22378124359616));
#21469=CARTESIAN_POINT('Ctrl Pts',(90.8844598705407,1.26974529951079,1.24216362930097));
#21470=CARTESIAN_POINT('Ctrl Pts',(90.8853060493219,1.26088025957503,1.25116128626806));
#21471=CARTESIAN_POINT('Ctrl Pts',(90.887256105412,1.24033525575579,1.2715735169381));
#21472=CARTESIAN_POINT('Ctrl Pts',(90.8883627645017,1.22859247399894,1.28292293500371));
#21473=CARTESIAN_POINT('Ctrl Pts',(90.8919891849614,1.18985457306871,1.31934354300732));
#21474=CARTESIAN_POINT('Ctrl Pts',(90.8945373036121,1.1622372349487,1.34373566898384));
#21475=CARTESIAN_POINT('Ctrl Pts',(90.9063805092729,1.032150039759,1.4516191454765));
#21476=CARTESIAN_POINT('Ctrl Pts',(90.9160771373006,0.921330794638997,1.52435925063414));
#21477=CARTESIAN_POINT('Ctrl Pts',(90.93099899312,0.739186450119857,1.61674580883643));
#21478=CARTESIAN_POINT('Ctrl Pts',(90.9362311828995,0.672944713849992,1.64542123656831));
#21479=CARTESIAN_POINT('Ctrl Pts',(90.9425284677456,0.588498383117651,1.67602115709609));
#21480=CARTESIAN_POINT('Ctrl Pts',(90.9437581926369,0.571769534773552,1.68180169016051));
#21481=CARTESIAN_POINT('Ctrl Pts',(90.9455741910302,0.546667400371461,1.69005767768158));
#21482=CARTESIAN_POINT('Ctrl Pts',(90.9461705704884,0.538358297206668,1.69272282211189));
#21483=CARTESIAN_POINT('Ctrl Pts',(90.9471961941674,0.523949119784549,1.6972277305699));
#21484=CARTESIAN_POINT('Ctrl Pts',(90.9476270477855,0.517858496607324,1.69909600371066));
#21485=CARTESIAN_POINT('Ctrl Pts',(90.9486401843571,0.50344874769937,1.70343145090378));
#21486=CARTESIAN_POINT('Ctrl Pts',(90.9492208410614,0.495121439469026,1.70587048675016));
#21487=CARTESIAN_POINT('Ctrl Pts',(90.9509465355028,0.470179782390178,1.71297777217132));
#21488=CARTESIAN_POINT('Ctrl Pts',(90.9520818175481,0.45351438768808,1.71746517586375));
#21489=CARTESIAN_POINT('Ctrl Pts',(90.9602738922053,0.331626561716199,1.74838725852858));
#21490=CARTESIAN_POINT('Ctrl Pts',(90.9669005649932,0.224230021972518,1.76537852957928));
#21491=CARTESIAN_POINT('Ctrl Pts',(90.9808220935346,-0.00210002200388923,
1.78018349565924));
#21492=CARTESIAN_POINT('Ctrl Pts',(90.9880994087397,-0.120603365252351,
1.77609345000407));
#21493=CARTESIAN_POINT('Ctrl Pts',(90.9972513888182,-0.260609268790078,
1.75717841661155));
#21494=CARTESIAN_POINT('Ctrl Pts',(90.9987541378413,-0.283341821030742,
1.75365632660867));
#21495=CARTESIAN_POINT('Ctrl Pts',(91.0011893501169,-0.319722864929306,
1.74729375446312));
#21496=CARTESIAN_POINT('Ctrl Pts',(91.0021129656754,-0.333417927353208,
1.7447322550437));
#21497=CARTESIAN_POINT('Ctrl Pts',(91.0038904278634,-0.359566695792879,
1.73952232863774));
#21498=CARTESIAN_POINT('Ctrl Pts',(91.0047433728787,-0.372024878531452,
1.73690057738642));
#21499=CARTESIAN_POINT('Ctrl Pts',(91.0067085270168,-0.400516029671903,
1.73058419533377));
#21500=CARTESIAN_POINT('Ctrl Pts',(91.0078235327917,-0.416527790364592,
1.72680031134141));
#21501=CARTESIAN_POINT('Ctrl Pts',(91.0114783602131,-0.468497957886142,
1.71375390604744));
#21502=CARTESIAN_POINT('Ctrl Pts',(91.0140467350314,-0.504216833483936,
1.70358675040614));
#21503=CARTESIAN_POINT('Ctrl Pts',(91.0258129536839,-0.66418587079092,1.65258098695349));
#21504=CARTESIAN_POINT('Ctrl Pts',(91.0353968911163,-0.783999239892148,
1.59921925682782));
#21505=CARTESIAN_POINT('Ctrl Pts',(91.0501408458299,-0.958411538080903,
1.49719668595346));
#21506=CARTESIAN_POINT('Ctrl Pts',(91.0553093936267,-1.01775421874025,1.45750776177013));
#21507=CARTESIAN_POINT('Ctrl Pts',(91.0615464072451,-1.08862420808789,1.40366435983973));
#21508=CARTESIAN_POINT('Ctrl Pts',(91.062773776462,-1.102534701564,1.39276472971141));
#21509=CARTESIAN_POINT('Ctrl Pts',(91.0645907447932,-1.12310526886498,1.37614519228709));
#21510=CARTESIAN_POINT('Ctrl Pts',(91.0651902598137,-1.12988891792469,1.37058092667042));
#21511=CARTESIAN_POINT('Ctrl Pts',(91.0662214400196,-1.14155519739722,1.36086621361119));
#21512=CARTESIAN_POINT('Ctrl Pts',(91.0666547216233,-1.14645689026059,1.35673937159642));
#21513=CARTESIAN_POINT('Ctrl Pts',(91.0676744828321,-1.15799256532709,1.34692007445035));
#21514=CARTESIAN_POINT('Ctrl Pts',(91.0682593135512,-1.16460699039142,1.34120506795032));
#21515=CARTESIAN_POINT('Ctrl Pts',(91.07000889991,-1.18438009603199,1.32386409729363));
#21516=CARTESIAN_POINT('Ctrl Pts',(91.0711635170415,-1.19740928661618,1.31209123819717));
#21517=CARTESIAN_POINT('Ctrl Pts',(91.0810075772964,-1.30807008317365,1.20907927089604));
#21518=CARTESIAN_POINT('Ctrl Pts',(91.0890477692518,-1.39530515361664,1.10727307526567));
#21519=CARTESIAN_POINT('Ctrl Pts',(91.1026245749139,-1.51895616421602,0.924854279858832));
#21520=CARTESIAN_POINT('Ctrl Pts',(91.1080248078927,-1.56228351631279,0.849618165046805));
#21521=CARTESIAN_POINT('Ctrl Pts',(91.1153014577173,-1.61127777820839,0.748016782202922));
#21522=CARTESIAN_POINT('Ctrl Pts',(91.1170009637716,-1.62209375827819,0.72426301186416));
#21523=CARTESIAN_POINT('Ctrl Pts',(91.1196765795121,-1.63812370243641,0.686896567880262));
#21524=CARTESIAN_POINT('Ctrl Pts',(91.1206403445507,-1.64370036256524,0.673442838195278));
#21525=CARTESIAN_POINT('Ctrl Pts',(91.1224484752508,-1.65379220488112,0.64822386283719));
#21526=CARTESIAN_POINT('Ctrl Pts',(91.1232913756476,-1.65834886571468,0.636476125820999));
#21527=CARTESIAN_POINT('Ctrl Pts',(91.1251884143469,-1.66827195313591,0.610062792260358));
#21528=CARTESIAN_POINT('Ctrl Pts',(91.126244737964,-1.67357067726382,0.595373060460751));
#21529=CARTESIAN_POINT('Ctrl Pts',(91.1289750988566,-1.68668371149883,0.557460688465905));
#21530=CARTESIAN_POINT('Ctrl Pts',(91.1306583184987,-1.69421222029347,0.534143436105127));
#21531=CARTESIAN_POINT('Ctrl Pts',(91.1403000899471,-1.73419655206887,0.400941197229571));
#21532=CARTESIAN_POINT('Ctrl Pts',(91.1485802151878,-1.75643712083253,0.288291544750243));
#21533=CARTESIAN_POINT('Ctrl Pts',(91.1625186589797,-1.77514871567458,0.0985316822635118));
#21534=CARTESIAN_POINT('Ctrl Pts',(91.1681042828945,-1.77774089524666,0.0223536772101882));
#21535=CARTESIAN_POINT('Ctrl Pts',(91.1754304370838,-1.77464885383945,-0.079765291498497));
#21536=CARTESIAN_POINT('Ctrl Pts',(91.1772803545186,-1.77328999568864,-0.105753436881783));
#21537=CARTESIAN_POINT('Ctrl Pts',(91.1804285438643,-1.76996541504043,-0.150467698956513));
#21538=CARTESIAN_POINT('Ctrl Pts',(91.1817375241805,-1.76827214033286,-0.169209359045446));
#21539=CARTESIAN_POINT('Ctrl Pts',(91.1836488818063,-1.76533162411925,-0.196847385115945));
#21540=CARTESIAN_POINT('Ctrl Pts',(91.184262749798,-1.76431428960216,-0.205766208150988));
#21541=CARTESIAN_POINT('Ctrl Pts',(91.185355345103,-1.76237147708351,-0.221723303105304));
#21542=CARTESIAN_POINT('Ctrl Pts',(91.185835408436,-1.76147137713992,-0.228764155432254));
#21543=CARTESIAN_POINT('Ctrl Pts',(91.1869089823393,-1.75935355041328,-0.244576276104114));
#21544=CARTESIAN_POINT('Ctrl Pts',(91.1875011917161,-1.75811241872631,-0.253344038158499));
#21545=CARTESIAN_POINT('Ctrl Pts',(91.1892998221417,-1.75412098211091,-0.28009762437475));
#21546=CARTESIAN_POINT('Ctrl Pts',(91.1904952089221,-1.75115976344716,-0.298051413525627));
#21547=CARTESIAN_POINT('Ctrl Pts',(91.197344592085,-1.7324262782389,-0.401687832087028));
#21548=CARTESIAN_POINT('Ctrl Pts',(91.2027297192348,-1.71064128653493,-0.486172733150881));
#21549=CARTESIAN_POINT('Ctrl Pts',(91.2132249058077,-1.65597225645751,-0.647926919155193));
#21550=CARTESIAN_POINT('Ctrl Pts',(91.2183254886979,-1.62364639111528,-0.725138034746177));
#21551=CARTESIAN_POINT('Ctrl Pts',(91.2273611868068,-1.55857906432791,-0.854169454192178));
#21552=CARTESIAN_POINT('Ctrl Pts',(91.2312294257906,-1.52837645285302,-0.90710440496241));
#21553=CARTESIAN_POINT('Ctrl Pts',(91.2364776654948,-1.48487942067013,-0.974979942292468));
#21554=CARTESIAN_POINT('Ctrl Pts',(91.2377707343639,-1.47396634509887,-0.991401000757056));
#21555=CARTESIAN_POINT('Ctrl Pts',(91.2399485013833,-1.45527836540388,-1.01853027896938));
#21556=CARTESIAN_POINT('Ctrl Pts',(91.2408275083637,-1.44765290318997,-1.02933964547821));
#21557=CARTESIAN_POINT('Ctrl Pts',(91.2425716951597,-1.43236502743538,-1.0505048412973));
#21558=CARTESIAN_POINT('Ctrl Pts',(91.2434365811453,-1.42470927311038,-1.06086448961843));
#21559=CARTESIAN_POINT('Ctrl Pts',(91.245361652411,-1.40750810549772,-1.08361880545344));
#21560=CARTESIAN_POINT('Ctrl Pts',(91.2464238557884,-1.39791034918522,-1.0959723586013));
#21561=CARTESIAN_POINT('Ctrl Pts',(91.2501469784148,-1.36390926762477,-1.13856282315742));
#21562=CARTESIAN_POINT('Ctrl Pts',(91.2528405448028,-1.33867953992551,-1.16812262851464));
#21563=CARTESIAN_POINT('Ctrl Pts',(91.2646089437274,-1.22582337815656,-1.29188628180531));
#21564=CARTESIAN_POINT('Ctrl Pts',(91.2740474102044,-1.12908387016809,-1.37723409169065));
#21565=CARTESIAN_POINT('Ctrl Pts',(91.2885987568033,-0.966196861288616,
-1.49215673627703));
#21566=CARTESIAN_POINT('Ctrl Pts',(91.2937255126596,-0.906005389609694,
-1.52945227319384));
#21567=CARTESIAN_POINT('Ctrl Pts',(91.2999162989816,-0.828269812292595,
-1.57141414748713));
#21568=CARTESIAN_POINT('Ctrl Pts',(91.3011378243745,-0.812671205839852,
-1.57953755085097));
#21569=CARTESIAN_POINT('Ctrl Pts',(91.3029464755025,-0.789146324290969,
-1.59134800155561));
#21570=CARTESIAN_POINT('Ctrl Pts',(91.3035434700806,-0.78130981805221,-1.59521013021559));
#21571=CARTESIAN_POINT('Ctrl Pts',(91.3045709630611,-0.767692545719014,
-1.60179681907707));
#21572=CARTESIAN_POINT('Ctrl Pts',(91.3050030627059,-0.761925263122236,
-1.60454815791507));
#21573=CARTESIAN_POINT('Ctrl Pts',(91.3060207313517,-0.748246150753339,
-1.61098352616868));
#21574=CARTESIAN_POINT('Ctrl Pts',(91.3066046484938,-0.740321869038026,
-1.61464044355246));
#21575=CARTESIAN_POINT('Ctrl Pts',(91.3083504580245,-0.716414239633213,
-1.62546038392408));
#21576=CARTESIAN_POINT('Ctrl Pts',(91.309502253525,-0.700351052286214,-1.63244579779591));
#21577=CARTESIAN_POINT('Ctrl Pts',(91.31936204865,-0.560615594713262,-1.69077030085083));
#21578=CARTESIAN_POINT('Ctrl Pts',(91.3274167848657,-0.431591433690345,
-1.72821673450586));
#21579=CARTESIAN_POINT('Ctrl Pts',(91.3410055552292,-0.214161570667849,
-1.76541974707872));
#21580=CARTESIAN_POINT('Ctrl Pts',(91.346401617071,-0.127808459809235,-1.77376283747623));
#21581=CARTESIAN_POINT('Ctrl Pts',(91.3536733281398,-0.0151143994283971,
-1.77637729589402));
#21582=CARTESIAN_POINT('Ctrl Pts',(91.3553722371953,0.0109774259569875,
-1.77640764595333));
#21583=CARTESIAN_POINT('Ctrl Pts',(91.3580469835552,0.0516160836335758,
-1.77555958264593));
#21584=CARTESIAN_POINT('Ctrl Pts',(91.3590104801715,0.0661680972872522,
-1.77507684715068));
#21585=CARTESIAN_POINT('Ctrl Pts',(91.3608181354188,0.0932968062942999,
-1.773842853534));
#21586=CARTESIAN_POINT('Ctrl Pts',(91.3616608294583,0.105874702123737,-1.77313657015911));
#21587=CARTESIAN_POINT('Ctrl Pts',(91.3635574396542,0.134022029597899,-1.77125546572881));
#21588=CARTESIAN_POINT('Ctrl Pts',(91.3646135409346,0.149585457152417,-1.77000903757965));
#21589=CARTESIAN_POINT('Ctrl Pts',(91.3673434427241,0.189522100166671,-1.76628015817118));
#21590=CARTESIAN_POINT('Ctrl Pts',(91.3690264243102,0.21386334589933,-1.76349839490747));
#21591=CARTESIAN_POINT('Ctrl Pts',(91.3786075067603,0.350818407721299,-1.74496983218926));
#21592=CARTESIAN_POINT('Ctrl Pts',(91.3868217643885,0.461756225916469,-1.71894342012451));
#21593=CARTESIAN_POINT('Ctrl Pts',(91.4007270838061,0.641979138753719,-1.65794853929313));
#21594=CARTESIAN_POINT('Ctrl Pts',(91.4063461578826,0.712868366638673,-1.62872655169136));
#21595=CARTESIAN_POINT('Ctrl Pts',(91.4137106856654,0.805088233832541,-1.58353344145636));
#21596=CARTESIAN_POINT('Ctrl Pts',(91.4155663519107,0.828269702049839,-1.57153258576421));
#21597=CARTESIAN_POINT('Ctrl Pts',(91.418723233832,0.867731944495391,-1.54998741662749));
#21598=CARTESIAN_POINT('Ctrl Pts',(91.4200352228598,0.884140340749637,-1.54068674559509));
#21599=CARTESIAN_POINT('Ctrl Pts',(91.4219502136567,0.908144372133074,-1.52657086746632));
#21600=CARTESIAN_POINT('Ctrl Pts',(91.4225647562539,0.91585599019513,-1.52195684171674));
#21601=CARTESIAN_POINT('Ctrl Pts',(91.4236583073059,0.929599408262028,-1.51359157211002));
#21602=CARTESIAN_POINT('Ctrl Pts',(91.4241386558857,0.935644085722084,-1.50986246285927));
#21603=CARTESIAN_POINT('Ctrl Pts',(91.4252126553516,0.949176472692837,-1.50140152253524));
#21604=CARTESIAN_POINT('Ctrl Pts',(91.4258050071342,0.956651334779626,-1.49664983887793));
#21605=CARTESIAN_POINT('Ctrl Pts',(91.4276031406114,0.979363596454923,-1.48197223093913));
#21606=CARTESIAN_POINT('Ctrl Pts',(91.4287979145563,0.994484913052898,-1.4718677141785));
#21607=CARTESIAN_POINT('Ctrl Pts',(91.4358963299324,1.08428866150907,-1.40984218554888));
#21608=CARTESIAN_POINT('Ctrl Pts',(91.441506083376,1.15505690375489,-1.35247345616729));
#21609=CARTESIAN_POINT('Ctrl Pts',(91.4545791935594,1.30958876101723,-1.20618419841582));
#21610=CARTESIAN_POINT('Ctrl Pts',(91.4620087480821,1.38919431205177,-1.11357029454688));
#21611=CARTESIAN_POINT('Ctrl Pts',(91.4717593981496,1.4758604047627,-0.988840260840585));
#21612=CARTESIAN_POINT('Ctrl Pts',(91.4737110491638,1.49239431445975,-0.963705367367069));
#21613=CARTESIAN_POINT('Ctrl Pts',(91.4766942346479,1.51638898607544,-0.925129256983195));
#21614=CARTESIAN_POINT('Ctrl Pts',(91.4777082113679,1.52432712609382,-0.911990398599405));
#21615=CARTESIAN_POINT('Ctrl Pts',(91.4794834949495,1.53784204527992,-0.888951612777335));
#21616=CARTESIAN_POINT('Ctrl Pts',(91.4802419401809,1.54349605317321,-0.87909786122651));
#21617=CARTESIAN_POINT('Ctrl Pts',(91.4819631056009,1.55605438883789,-0.85671663679039));
#21618=CARTESIAN_POINT('Ctrl Pts',(91.4829277735815,1.56290262352812,-0.844158767808961));
#21619=CARTESIAN_POINT('Ctrl Pts',(91.4855404856088,1.58093549419929,-0.810119457861819));
#21620=CARTESIAN_POINT('Ctrl Pts',(91.4871984411343,1.59183333756537,-0.788490391335275));
#21621=CARTESIAN_POINT('Ctrl Pts',(91.4989289802033,1.66511590629817,-0.635330338555039));
#21622=CARTESIAN_POINT('Ctrl Pts',(91.509555776627,1.71155443579279,-0.496810776419606));
#21623=CARTESIAN_POINT('Ctrl Pts',(91.5243665717549,1.75197377673693,-0.298194959594751));
#21624=CARTESIAN_POINT('Ctrl Pts',(91.5285278224775,1.76066374846439,-0.241653201940884));
#21625=CARTESIAN_POINT('Ctrl Pts',(91.5349198382908,1.7699848913351,-0.152541081512852));
#21626=CARTESIAN_POINT('Ctrl Pts',(91.537205049005,1.77247461432816,-0.12020546207983));
#21627=CARTESIAN_POINT('Ctrl Pts',(91.5402117281035,1.77462319028804,-0.0768002173295743));
#21628=CARTESIAN_POINT('Ctrl Pts',(91.5409700025633,1.77506592803839,-0.0657777142948062));
#21629=CARTESIAN_POINT('Ctrl Pts',(91.541886871471,1.77548006742821,-0.052348562860265));
#21630=CARTESIAN_POINT('Ctrl Pts',(91.5420506674495,1.7755492920597,-0.0499455056259374));
#21631=CARTESIAN_POINT('Ctrl Pts',(91.5422141974348,1.77561363837091,-0.0475422941309033));
#21632=CARTESIAN_POINT('Origin',(88.3562164250559,0.,0.));
#21633=CARTESIAN_POINT('',(92.4397243119761,1.77561363837197,-0.0475422940913782));
#21634=CARTESIAN_POINT('',(92.2900876926257,1.77561363857513,-0.047542286503657));
#21635=CARTESIAN_POINT('',(88.3562164250559,1.77561363837197,-0.0475422940912398));
#21636=CARTESIAN_POINT('',(92.4397193140361,1.77561154215721,-0.047620519296831));
#21637=CARTESIAN_POINT('Ctrl Pts',(92.4397243119761,1.77561363837196,-0.0475422940915214));
#21638=CARTESIAN_POINT('Ctrl Pts',(92.4397224335513,1.77561285117158,-0.0475716945183764));
#21639=CARTESIAN_POINT('Ctrl Pts',(92.4397211924972,1.77561233065394,-0.0475911188635325));
#21640=CARTESIAN_POINT('Ctrl Pts',(92.4397193140361,1.77561154215721,-0.0476205192968057));
#21641=CARTESIAN_POINT('Ctrl Pts',(92.4397193140361,1.77561154215721,-0.0476205192967044));
#21642=CARTESIAN_POINT('Ctrl Pts',(92.4384162706077,1.77506458088494,-0.0680148947152969));
#21643=CARTESIAN_POINT('Ctrl Pts',(92.4371048348684,1.77416680544134,-0.0883877160786648));
#21644=CARTESIAN_POINT('Ctrl Pts',(92.4347613706043,1.77195318636845,-0.124475693326451));
#21645=CARTESIAN_POINT('Ctrl Pts',(92.4337342110471,1.77077941231963,-0.140187519064086));
#21646=CARTESIAN_POINT('Ctrl Pts',(92.4318637772838,1.76827725088801,-0.168589370914655));
#21647=CARTESIAN_POINT('Ctrl Pts',(92.4310227541361,1.76702083497391,-0.181284766744872));
#21648=CARTESIAN_POINT('Ctrl Pts',(92.4293764235636,1.76430771801814,-0.205981739748837));
#21649=CARTESIAN_POINT('Ctrl Pts',(92.4285715967944,1.76286502317096,-0.217984170741241));
#21650=CARTESIAN_POINT('Ctrl Pts',(92.4268572589327,1.75954733667217,-0.243393674222738));
#21651=CARTESIAN_POINT('Ctrl Pts',(92.4259468177277,1.75764136986009,-0.256795848774373));
#21652=CARTESIAN_POINT('Ctrl Pts',(92.4236283969233,1.75242632634737,-0.290682966275401));
#21653=CARTESIAN_POINT('Ctrl Pts',(92.422213995457,1.74891120659691,-0.311133643018388));
#21654=CARTESIAN_POINT('Ctrl Pts',(92.4162767462431,1.73278400641467,-0.396023898322558));
#21655=CARTESIAN_POINT('Ctrl Pts',(92.411654521346,1.7169634042702,-0.459793615133651));
#21656=CARTESIAN_POINT('Ctrl Pts',(92.4021046474298,1.67778014761543,-0.587095150418172));
#21657=CARTESIAN_POINT('Ctrl Pts',(92.3971795864593,1.65424325619602,-0.650465327122878));
#21658=CARTESIAN_POINT('Ctrl Pts',(92.3870494763906,1.59869069907259,-0.777361262422159));
#21659=CARTESIAN_POINT('Ctrl Pts',(92.3818517147233,1.56635116142991,-0.840623247298179));
#21660=CARTESIAN_POINT('Ctrl Pts',(92.3741186200029,1.51154005078284,-0.933636861374367));
#21661=CARTESIAN_POINT('Ctrl Pts',(92.3715033217727,1.49177731797006,-0.964899991260372));
#21662=CARTESIAN_POINT('Ctrl Pts',(92.3681370516592,1.46454397456659,-1.0051416930856));
#21663=CARTESIAN_POINT('Ctrl Pts',(92.3673380194824,1.45794209507266,-1.01469391551458));
#21664=CARTESIAN_POINT('Ctrl Pts',(92.3660301905661,1.44690034856385,-1.03033987932306));
#21665=CARTESIAN_POINT('Ctrl Pts',(92.3655179241297,1.44251460618257,-1.03647117820593));
#21666=CARTESIAN_POINT('Ctrl Pts',(92.3645510806996,1.43411867500942,-1.04805222363226));
#21667=CARTESIAN_POINT('Ctrl Pts',(92.3640959731004,1.43011616954989,-1.05350727712053));
#21668=CARTESIAN_POINT('Ctrl Pts',(92.3628748512699,1.41924380007105,-1.06814918703678));
#21669=CARTESIAN_POINT('Ctrl Pts',(92.3621127479233,1.41231581214442,-1.07729277073242));
#21670=CARTESIAN_POINT('Ctrl Pts',(92.3591889681092,1.38520712231163,-1.1123598907171));
#21671=CARTESIAN_POINT('Ctrl Pts',(92.3570665068653,1.36439604486501,-1.13779042438384));
#21672=CARTESIAN_POINT('Ctrl Pts',(92.3483628942292,1.2749303647725,-1.24112724157452));
#21673=CARTESIAN_POINT('Ctrl Pts',(92.3420620211534,1.20021345764129,-1.31352028679284));
#21674=CARTESIAN_POINT('Ctrl Pts',(92.3299537090243,1.04735027494071,-1.43763036408985));
#21675=CARTESIAN_POINT('Ctrl Pts',(92.3241814717585,0.970616776156143,-1.49051130918445));
#21676=CARTESIAN_POINT('Ctrl Pts',(92.3164452519067,0.86671287661616,-1.55067830307281));
#21677=CARTESIAN_POINT('Ctrl Pts',(92.3146870482974,0.843021022140021,-1.5636846997781));
#21678=CARTESIAN_POINT('Ctrl Pts',(92.311933916625,0.805875972799583,-1.58298709867434));
#21679=CARTESIAN_POINT('Ctrl Pts',(92.3109524128512,0.792624410471672,-1.58966372531649));
#21680=CARTESIAN_POINT('Ctrl Pts',(92.3091191482691,0.767867302141811,-1.60175075424609));
#21681=CARTESIAN_POINT('Ctrl Pts',(92.3082689936447,0.756384235853919,-1.60720519712905));
#21682=CARTESIAN_POINT('Ctrl Pts',(92.3063659496786,0.730681675707032,-1.6190774261403));
#21683=CARTESIAN_POINT('Ctrl Pts',(92.3053109631407,0.716434333570718,-1.62543201691363));
#21684=CARTESIAN_POINT('Ctrl Pts',(92.3026042941029,0.679895886453454,-1.64115515855599));
#21685=CARTESIAN_POINT('Ctrl Pts',(92.3009438184613,0.657494423553019,-1.65025745075125));
#21686=CARTESIAN_POINT('Ctrl Pts',(92.2905656268471,0.517623478910721,-1.70379064120068));
#21687=CARTESIAN_POINT('Ctrl Pts',(92.2814529765301,0.395921060732133,-1.7361084800252));
#21688=CARTESIAN_POINT('Ctrl Pts',(92.267278649882,0.20439943424351,-1.7657701042476));
#21689=CARTESIAN_POINT('Ctrl Pts',(92.2622855257097,0.136396408661462,-1.77232054561005));
#21690=CARTESIAN_POINT('Ctrl Pts',(92.2548117718038,0.0320607790416382,
-1.77632847661682));
#21691=CARTESIAN_POINT('Ctrl Pts',(92.2522564444011,-0.00409766566065642,
-1.77661317659523));
#21692=CARTESIAN_POINT('Ctrl Pts',(92.2489541773622,-0.0517623354439688,
-1.77553301907567));
#21693=CARTESIAN_POINT('Ctrl Pts',(92.2481613400909,-0.0632799178735311,
-1.77515985504275));
#21694=CARTESIAN_POINT('Ctrl Pts',(92.2468609329884,-0.0823066235505851,
-1.77435797699596));
#21695=CARTESIAN_POINT('Ctrl Pts',(92.2463499683301,-0.0898179543904061,
-1.77399361690382));
#21696=CARTESIAN_POINT('Ctrl Pts',(92.2453833914227,-0.104098400217065,
-1.77320996382178));
#21697=CARTESIAN_POINT('Ctrl Pts',(92.2449272701061,-0.110867781690771,
-1.7727995914977));
#21698=CARTESIAN_POINT('Ctrl Pts',(92.2436995390321,-0.129165743014583,
-1.77158511563581));
#21699=CARTESIAN_POINT('Ctrl Pts',(92.2429319165576,-0.140689334039717,
-1.77070724290043));
#21700=CARTESIAN_POINT('Ctrl Pts',(92.2399587098838,-0.185606528062117,
-1.76684415461661));
#21701=CARTESIAN_POINT('Ctrl Pts',(92.2377940490086,-0.218923658287862,
-1.76302604027329));
#21702=CARTESIAN_POINT('Ctrl Pts',(92.2290880227354,-0.35436489857077,-1.74360533218544));
#21703=CARTESIAN_POINT('Ctrl Pts',(92.2228194346928,-0.455149079117714,
-1.72005141200978));
#21704=CARTESIAN_POINT('Ctrl Pts',(92.2107594851322,-0.641495395311842,
-1.65896291784003));
#21705=CARTESIAN_POINT('Ctrl Pts',(92.2050028075449,-0.72725959327133,-1.62319593042249));
#21706=CARTESIAN_POINT('Ctrl Pts',(92.1972855347556,-0.833855371826907,
-1.56859102934989));
#21707=CARTESIAN_POINT('Ctrl Pts',(92.1955294564356,-0.857593521728362,
-1.5557396390121));
#21708=CARTESIAN_POINT('Ctrl Pts',(92.1927789247224,-0.893907181450863,
-1.53499641293168));
#21709=CARTESIAN_POINT('Ctrl Pts',(92.1917978537178,-0.906692706365165,
-1.5274790835144));
#21710=CARTESIAN_POINT('Ctrl Pts',(92.1899649883115,-0.930259828558774,
-1.51322249990443));
#21711=CARTESIAN_POINT('Ctrl Pts',(92.1891147944941,-0.941066170781586,
-1.50652584795496));
#21712=CARTESIAN_POINT('Ctrl Pts',(92.1872111332242,-0.964977858574336,
-1.49135019931309));
#21713=CARTESIAN_POINT('Ctrl Pts',(92.1861555619857,-0.978045060928342,
-1.48281337873496));
#21714=CARTESIAN_POINT('Ctrl Pts',(92.1834463158229,-1.01108734797192,-1.46060002531754));
#21715=CARTESIAN_POINT('Ctrl Pts',(92.1817838188473,-1.03089788655939,-1.44668569710708));
#21716=CARTESIAN_POINT('Ctrl Pts',(92.1714366396688,-1.15130334514369,-1.35838740749496));
#21717=CARTESIAN_POINT('Ctrl Pts',(92.1623604611292,-1.24407428406101,-1.27396411046387));
#21718=CARTESIAN_POINT('Ctrl Pts',(92.1481988293956,-1.37276474707537,-1.12928405745019));
#21719=CARTESIAN_POINT('Ctrl Pts',(92.1431824620932,-1.41533280276073,-1.07545316019012));
#21720=CARTESIAN_POINT('Ctrl Pts',(92.1356791453553,-1.47548174532882,-0.989611672438018));
#21721=CARTESIAN_POINT('Ctrl Pts',(92.1331169037432,-1.49536823517074,-0.959297611233721));
#21722=CARTESIAN_POINT('Ctrl Pts',(92.129807246919,-1.52034270328216,-0.918561452719356));
#21723=CARTESIAN_POINT('Ctrl Pts',(92.1290136870216,-1.52627508130396,-0.90867016669605));
#21724=CARTESIAN_POINT('Ctrl Pts',(92.1277124146958,-1.53591675303896,-0.892233360974677));
#21725=CARTESIAN_POINT('Ctrl Pts',(92.1272012987223,-1.5396814794406,-0.885720944473918));
#21726=CARTESIAN_POINT('Ctrl Pts',(92.1261712376869,-1.54722530287246,-0.872477794520266));
#21727=CARTESIAN_POINT('Ctrl Pts',(92.1256524343739,-1.55100210368083,-0.865745990399245));
#21728=CARTESIAN_POINT('Ctrl Pts',(92.1243036408515,-1.56075713798443,-0.848089789612762));
#21729=CARTESIAN_POINT('Ctrl Pts',(92.1234779701487,-1.5666647051273,-0.837126548687118));
#21730=CARTESIAN_POINT('Ctrl Pts',(92.1199010174589,-1.59194656589751,-0.78900338062029));
#21731=CARTESIAN_POINT('Ctrl Pts',(92.1172148760661,-1.6101192078813,-0.751223636607381));
#21732=CARTESIAN_POINT('Ctrl Pts',(92.1084501943705,-1.66587078188128,-0.623978655682495));
#21733=CARTESIAN_POINT('Ctrl Pts',(92.1025620093898,-1.69745960757359,-0.532078969323977));
#21734=CARTESIAN_POINT('Ctrl Pts',(92.0910776878918,-1.74347711518394,-0.351247802887306));
#21735=CARTESIAN_POINT('Ctrl Pts',(92.0855099249027,-1.7589674342231,-0.262903850354378));
#21736=CARTESIAN_POINT('Ctrl Pts',(92.0780227141735,-1.77032938296649,-0.147323908230554));
#21737=CARTESIAN_POINT('Ctrl Pts',(92.0762928336041,-1.77233546264824,-0.120819476066508));
#21738=CARTESIAN_POINT('Ctrl Pts',(92.0735743674978,-1.77452885493572,-0.0795543536124082));
#21739=CARTESIAN_POINT('Ctrl Pts',(92.0725986530132,-1.77512817862992,-0.0648188210614253));
#21740=CARTESIAN_POINT('Ctrl Pts',(92.0707706890069,-1.77590251252812,-0.0373643176233218));
#21741=CARTESIAN_POINT('Ctrl Pts',(92.0699199705932,-1.77612451990107,-0.0246475458464306));
#21742=CARTESIAN_POINT('Ctrl Pts',(92.0680084594704,-1.77631548099647,0.00378444383170876));
#21743=CARTESIAN_POINT('Ctrl Pts',(92.0669454794358,-1.77621248026179,0.0194989044897602));
#21744=CARTESIAN_POINT('Ctrl Pts',(92.0642034855025,-1.77541391757267,0.0597769061715121));
#21745=CARTESIAN_POINT('Ctrl Pts',(92.0625152782607,-1.77441712425732,0.0843304295636668));
#21746=CARTESIAN_POINT('Ctrl Pts',(92.0528664235511,-1.76588863718058,0.223233950027916));
#21747=CARTESIAN_POINT('Ctrl Pts',(92.044584243175,-1.74781483915964,0.336647026443929));
#21748=CARTESIAN_POINT('Ctrl Pts',(92.0306709074447,-1.69985930938506,0.520850913337519));
#21749=CARTESIAN_POINT('Ctrl Pts',(92.025112149224,-1.67609131359707,0.592896423639816));
#21750=CARTESIAN_POINT('Ctrl Pts',(92.0169265218084,-1.63346964055078,0.698793715386502));
#21751=CARTESIAN_POINT('Ctrl Pts',(92.0142102350385,-1.61799578438501,0.733911340574197));
#21752=CARTESIAN_POINT('Ctrl Pts',(92.0107366429896,-1.59630998077861,0.77909990690063));
#21753=CARTESIAN_POINT('Ctrl Pts',(92.0099275351686,-1.59111931043537,0.789646489521547));
#21754=CARTESIAN_POINT('Ctrl Pts',(92.0086076132218,-1.58241495787134,0.806897912043264));
#21755=CARTESIAN_POINT('Ctrl Pts',(92.0080932070205,-1.57896251896122,0.813633031136685));
#21756=CARTESIAN_POINT('Ctrl Pts',(92.0071258091406,-1.57235359692246,0.826325404927407));
#21757=CARTESIAN_POINT('Ctrl Pts',(92.0066722527021,-1.56920607109502,0.832287101226458));
#21758=CARTESIAN_POINT('Ctrl Pts',(92.0054613674507,-1.56067364376164,0.848227806669165));
#21759=CARTESIAN_POINT('Ctrl Pts',(92.0047078318479,-1.55522689698367,0.858173612959993));
#21760=CARTESIAN_POINT('Ctrl Pts',(92.0018590678015,-1.53412877686555,0.895838270487618));
#21761=CARTESIAN_POINT('Ctrl Pts',(91.9998005364955,-1.51782759656934,0.923188491452394));
#21762=CARTESIAN_POINT('Ctrl Pts',(91.9910999242232,-1.44482855201506,1.03850089019707));
#21763=CARTESIAN_POINT('Ctrl Pts',(91.9847497337416,-1.38115017437794,1.12180285336836));
#21764=CARTESIAN_POINT('Ctrl Pts',(91.9725676513696,-1.2474138892642,1.26797382925055));
#21765=CARTESIAN_POINT('Ctrl Pts',(91.9667717445636,-1.17898821282085,1.33183446579999));
#21766=CARTESIAN_POINT('Ctrl Pts',(91.9590067018434,-1.08467317627199,1.40686931300259));
#21767=CARTESIAN_POINT('Ctrl Pts',(91.9572452735813,-1.06310318272823,1.42323879210941));
#21768=CARTESIAN_POINT('Ctrl Pts',(91.954488196641,-1.02913811600939,1.44781189456886));
#21769=CARTESIAN_POINT('Ctrl Pts',(91.9535060359196,-1.01699950088809,1.4563641497182));
#21770=CARTESIAN_POINT('Ctrl Pts',(91.9516721632255,-0.994272599941517,
1.47195368622833));
#21771=CARTESIAN_POINT('Ctrl Pts',(91.9508220659182,-0.98371315790604,1.47903146209307));
#21772=CARTESIAN_POINT('Ctrl Pts',(91.9489199497421,-0.960038605580013,
1.49453434400107));
#21773=CARTESIAN_POINT('Ctrl Pts',(91.9478658436122,-0.946886861040254,
1.50290128582479));
#21774=CARTESIAN_POINT('Ctrl Pts',(91.9451630555746,-0.913094508367213,
1.52377984036966));
#21775=CARTESIAN_POINT('Ctrl Pts',(91.9435056240067,-0.892306451459931,
1.53604546815214));
#21776=CARTESIAN_POINT('Ctrl Pts',(91.9330833336318,-0.761233467836146,
1.6098241072713));
#21777=CARTESIAN_POINT('Ctrl Pts',(91.9239185934707,-0.644917891274431,
1.65984346453568));
#21778=CARTESIAN_POINT('Ctrl Pts',(91.9097259041086,-0.45950959129633,1.71712390057367));
#21779=CARTESIAN_POINT('Ctrl Pts',(91.9047656930783,-0.393615351687797,
1.73341611071753));
#21780=CARTESIAN_POINT('Ctrl Pts',(91.8973338477697,-0.291550667199426,
1.75252936755916));
#21781=CARTESIAN_POINT('Ctrl Pts',(91.8947883560639,-0.255956960426443,
1.75808060841535));
#21782=CARTESIAN_POINT('Ctrl Pts',(91.8914966051869,-0.208796860709239,
1.76397289517714));
#21783=CARTESIAN_POINT('Ctrl Pts',(91.8907047988677,-0.197363344843533,
1.76528871060033));
#21784=CARTESIAN_POINT('Ctrl Pts',(91.8894056252635,-0.178441910814071,
1.76728012776684));
#21785=CARTESIAN_POINT('Ctrl Pts',(91.8888948755928,-0.170961204841223,
1.76801946792131));
#21786=CARTESIAN_POINT('Ctrl Pts',(91.8878647521115,-0.155783411864449,
1.76942229819417));
#21787=CARTESIAN_POINT('Ctrl Pts',(91.8873455279225,-0.148086286713316,
1.77008310488363));
#21788=CARTESIAN_POINT('Ctrl Pts',(91.8859943474189,-0.127941197248894,
1.77168025666717));
#21789=CARTESIAN_POINT('Ctrl Pts',(91.8851667387025,-0.115486991149258,
1.77253565793019));
#21790=CARTESIAN_POINT('Ctrl Pts',(91.8815657708556,-0.0608501975413613,
1.77570999332726));
#21791=CARTESIAN_POINT('Ctrl Pts',(91.8788586490298,-0.0185982483418953,
1.77665513193569));
#21792=CARTESIAN_POINT('Ctrl Pts',(91.8753622020439,0.0368335383901947,
1.77591699439609));
#21793=CARTESIAN_POINT('Ctrl Pts',(91.8745349087929,0.0500142549386234,
1.77559467993379));
#21794=CARTESIAN_POINT('Ctrl Pts',(91.8633664011248,0.228615926543652,1.769236870932));
#21795=CARTESIAN_POINT('Ctrl Pts',(91.8535216497016,0.392399803307351,1.74025550326595));
#21796=CARTESIAN_POINT('Ctrl Pts',(91.8409076018317,0.579477199565824,1.67935814700008));
#21797=CARTESIAN_POINT('Ctrl Pts',(91.8388853173912,0.608885385620271,1.66892061177424));
#21798=CARTESIAN_POINT('Ctrl Pts',(91.8358102077816,0.652613531539066,1.65209102623873));
#21799=CARTESIAN_POINT('Ctrl Pts',(91.8347764777623,0.667149585711418,1.64627475975517));
#21800=CARTESIAN_POINT('Ctrl Pts',(91.832891401069,0.693348504046896,1.63538790435042));
#21801=CARTESIAN_POINT('Ctrl Pts',(91.832042317579,0.705037526903719,1.63038272100396));
#21802=CARTESIAN_POINT('Ctrl Pts',(91.8301960411874,0.730207281430418,1.619283863412));
#21803=CARTESIAN_POINT('Ctrl Pts',(91.8291973974487,0.743667551081964,1.613146445466));
#21804=CARTESIAN_POINT('Ctrl Pts',(91.826423053717,0.780628225664122,1.59573275162663));
#21805=CARTESIAN_POINT('Ctrl Pts',(91.8246354112315,0.803958669644917,1.58410661673838));
#21806=CARTESIAN_POINT('Ctrl Pts',(91.8137524017066,0.943027524988194,1.51094165873883));
#21807=CARTESIAN_POINT('Ctrl Pts',(91.804224378576,1.0518998242969,1.43726843307516));
#21808=CARTESIAN_POINT('Ctrl Pts',(91.7898960501897,1.20105764586991,1.3102421806304));
#21809=CARTESIAN_POINT('Ctrl Pts',(91.7851561968135,1.24811641309629,1.26549608234068));
#21810=CARTESIAN_POINT('Ctrl Pts',(91.778006391002,1.31668748356836,1.19274018908559));
#21811=CARTESIAN_POINT('Ctrl Pts',(91.7755281503241,1.33999198730462,1.16649772817379));
#21812=CARTESIAN_POINT('Ctrl Pts',(91.7723084586074,1.36982345088723,1.13083061637614));
#21813=CARTESIAN_POINT('Ctrl Pts',(91.7715238242253,1.37705722589921,1.12201050948417));
#21814=CARTESIAN_POINT('Ctrl Pts',(91.7702332267552,1.38890327164627,1.10727952854062));
#21815=CARTESIAN_POINT('Ctrl Pts',(91.7697239675693,1.39356389600405,1.10140815653529));
#21816=CARTESIAN_POINT('Ctrl Pts',(91.7687576556362,1.40238357045093,1.09015167489518));
#21817=CARTESIAN_POINT('Ctrl Pts',(91.7683001229671,1.40654906076195,1.08477190992296));
#21818=CARTESIAN_POINT('Ctrl Pts',(91.767063260686,1.41777743064768,1.07009695738435));
#21819=CARTESIAN_POINT('Ctrl Pts',(91.7662880246245,1.42477990221484,1.06075566907453));
#21820=CARTESIAN_POINT('Ctrl Pts',(91.7632450834048,1.45209833828793,1.02355426970084));
#21821=CARTESIAN_POINT('Ctrl Pts',(91.7610207790669,1.4716947200969,0.995172317384239));
#21822=CARTESIAN_POINT('Ctrl Pts',(91.7523107378704,1.54623815049912,0.880186363919749));
#21823=CARTESIAN_POINT('Ctrl Pts',(91.7460874019661,1.59447016362826,0.789461020201902));
#21824=CARTESIAN_POINT('Ctrl Pts',(91.7388340402168,1.6406200505518,0.680930342919028));
#21825=CARTESIAN_POINT('Ctrl Pts',(91.7378874286032,1.64645047773804,0.666709156673473));
#21826=CARTESIAN_POINT('Ctrl Pts',(91.73202836253,1.68130427070451,0.578449586914254));
#21827=CARTESIAN_POINT('Ctrl Pts',(91.7270568303196,1.7055100168224,0.502614665240375));
#21828=CARTESIAN_POINT('Ctrl Pts',(91.7202765414743,1.73066470906533,0.400643118378392));
#21829=CARTESIAN_POINT('Ctrl Pts',(91.7186138959088,1.73624154998054,0.375739825724619));
#21830=CARTESIAN_POINT('Ctrl Pts',(91.7159777971819,1.74414879221804,0.336482057373719));
#21831=CARTESIAN_POINT('Ctrl Pts',(91.7150159437258,1.7468428323552,0.322203789946394));
#21832=CARTESIAN_POINT('Ctrl Pts',(91.7132001822935,1.75156970911691,0.295347131620639));
#21833=CARTESIAN_POINT('Ctrl Pts',(91.7123476225591,1.75364297393904,0.282776730647458));
#21834=CARTESIAN_POINT('Ctrl Pts',(91.7104134190957,1.75801711107587,0.254354945609482));
#21835=CARTESIAN_POINT('Ctrl Pts',(91.7093293507303,1.76023912703704,0.238492740923997));
#21836=CARTESIAN_POINT('Ctrl Pts',(91.7059806226956,1.76640065437399,0.189714765287039));
#21837=CARTESIAN_POINT('Ctrl Pts',(91.7036941703071,1.76963328852576,0.156718640754545));
#21838=CARTESIAN_POINT('Ctrl Pts',(91.697390069832,1.77592041452695,0.0666246359638738));
#21839=CARTESIAN_POINT('Ctrl Pts',(91.693324754067,1.77714075608374,0.0094926279344601));
#21840=CARTESIAN_POINT('Ctrl Pts',(91.6892085959652,1.77561363837197,-0.0475422940912359));
#21841=CARTESIAN_POINT('Ctrl Pts',(91.5422141974348,1.77561363837091,-0.0475422941309033));
#21842=CARTESIAN_POINT('Ctrl Pts',(91.5425519318852,1.77574653122244,-0.0425790006270345));
#21843=CARTESIAN_POINT('Ctrl Pts',(91.5428885299719,1.77585861629585,-0.0376150490231579));
#21844=CARTESIAN_POINT('Ctrl Pts',(91.5436822177452,1.7760745899505,-0.0258676734239604));
#21845=CARTESIAN_POINT('Ctrl Pts',(91.5441382891879,1.7761604350442,-0.0190839848731418));
#21846=CARTESIAN_POINT('Ctrl Pts',(91.5453824660129,1.77628917985943,-0.000492058207452863));
#21847=CARTESIAN_POINT('Ctrl Pts',(91.5461663296664,1.77625320414425,0.0113166306758942));
#21848=CARTESIAN_POINT('Ctrl Pts',(91.5493297410634,1.7756282768274,0.0593148228646064));
#21849=CARTESIAN_POINT('Ctrl Pts',(91.5516611592437,1.77405101696591,0.0954852307471094));
#21850=CARTESIAN_POINT('Ctrl Pts',(91.5629724388346,1.76084423229778,0.273272296370204));
#21851=CARTESIAN_POINT('Ctrl Pts',(91.5714485930022,1.73335746888836,0.413192838573033));
#21852=CARTESIAN_POINT('Ctrl Pts',(91.5843105432977,1.66973662378181,0.609210664155319));
#21853=CARTESIAN_POINT('Ctrl Pts',(91.588366794124,1.64671191933351,0.668951830668713));
#21854=CARTESIAN_POINT('Ctrl Pts',(91.5938323575766,1.61231893159721,0.745582024222819));
#21855=CARTESIAN_POINT('Ctrl Pts',(91.5951449262976,1.60381315424725,0.763706884215499));
#21856=CARTESIAN_POINT('Ctrl Pts',(91.5973467248221,1.58915207158709,0.793622408729495));
#21857=CARTESIAN_POINT('Ctrl Pts',(91.5982299959621,1.58316730546669,0.805494941522774));
#21858=CARTESIAN_POINT('Ctrl Pts',(91.599975952941,1.5711391266092,0.828704368234416));
#21859=CARTESIAN_POINT('Ctrl Pts',(91.6008382737704,1.56510487981056,0.840045109048163));
#21860=CARTESIAN_POINT('Ctrl Pts',(91.6027493051344,1.55153018224219,0.864903297216508));
#21861=CARTESIAN_POINT('Ctrl Pts',(91.6037999213665,1.54393505300273,0.878389518116582));
#21862=CARTESIAN_POINT('Ctrl Pts',(91.607461713061,1.51701486077285,0.924762068604568));
#21863=CARTESIAN_POINT('Ctrl Pts',(91.6101042527252,1.4968086475851,0.957121966447943));
#21864=CARTESIAN_POINT('Ctrl Pts',(91.621869423726,1.40351796854557,1.09633823509033));
#21865=CARTESIAN_POINT('Ctrl Pts',(91.6313641976844,1.31992734195272,1.19565996791369));
#21866=CARTESIAN_POINT('Ctrl Pts',(91.6459922333852,1.17495045547046,1.33401467858381));
#21867=CARTESIAN_POINT('Ctrl Pts',(91.6511376289472,1.1206960358983,1.37990799055999));
#21868=CARTESIAN_POINT('Ctrl Pts',(91.6573484360426,1.04972712866114,1.43298548217403));
#21869=CARTESIAN_POINT('Ctrl Pts',(91.6585722199366,1.0354620742978,1.44332698588431));
#21870=CARTESIAN_POINT('Ctrl Pts',(91.6603837958991,1.01388802678376,1.45848264611069));
#21871=CARTESIAN_POINT('Ctrl Pts',(91.6609814873964,1.00669396768641,1.46345748945314));
#21872=CARTESIAN_POINT('Ctrl Pts',(91.6620098489672,0.994178730341113,1.47197607964926));
#21873=CARTESIAN_POINT('Ctrl Pts',(91.6624421264867,0.988874878167424,1.47554444380408));
#21874=CARTESIAN_POINT('Ctrl Pts',(91.6634597697117,0.976287135375212,1.48391495698939));
#21875=CARTESIAN_POINT('Ctrl Pts',(91.6640434879078,0.968986993958848,1.48869217228892));
#21876=CARTESIAN_POINT('Ctrl Pts',(91.6657881620775,0.946938087578518,1.50289007578937));
#21877=CARTESIAN_POINT('Ctrl Pts',(91.6669390394554,0.932084515807071,1.51214709390441));
#21878=CARTESIAN_POINT('Ctrl Pts',(91.6768023363388,0.802366118897334,1.59035212828615));
#21879=CARTESIAN_POINT('Ctrl Pts',(91.6848606573189,0.680163382060995,1.64632902600288));
#21880=CARTESIAN_POINT('Ctrl Pts',(91.6984505274092,0.470514268804361,1.71498685779538));
#21881=CARTESIAN_POINT('Ctrl Pts',(91.7038436646326,0.38636335416173,1.73588147781375));
#21882=CARTESIAN_POINT('Ctrl Pts',(91.7111116468031,0.275327105440494,1.75497556409935));
#21883=CARTESIAN_POINT('Ctrl Pts',(91.7128099411117,0.249530971905259,1.75882870848304));
#21884=CARTESIAN_POINT('Ctrl Pts',(91.7154837934504,0.209220516165679,1.7639452110253));
#21885=CARTESIAN_POINT('Ctrl Pts',(91.7164470185801,0.19475902641779,1.76560041694032));
#21886=CARTESIAN_POINT('Ctrl Pts',(91.7182541990949,0.167749602095877,1.76835594772748));
#21887=CARTESIAN_POINT('Ctrl Pts',(91.7190966907885,0.155207068665014,1.76950090098788));
#21888=CARTESIAN_POINT('Ctrl Pts',(91.720992880387,0.127094315643159,1.77176600128456));
#21889=CARTESIAN_POINT('Ctrl Pts',(91.7220487633459,0.111519538705679,1.77281445551605));
#21890=CARTESIAN_POINT('Ctrl Pts',(91.7247781308554,0.0714756030363633,
1.77498034750434));
#21891=CARTESIAN_POINT('Ctrl Pts',(91.7264607959453,0.0469941918793711,
1.77579712742451));
#21892=CARTESIAN_POINT('Ctrl Pts',(91.7360700870387,-0.0916038404876299,
1.77755327864952));
#21893=CARTESIAN_POINT('Ctrl Pts',(91.7443155224906,-0.205567735304695,
1.7679990859125));
#21894=CARTESIAN_POINT('Ctrl Pts',(91.7582349886872,-0.392935650278824,
1.7339251046491));
#21895=CARTESIAN_POINT('Ctrl Pts',(91.7638366925282,-0.467105698121408,
1.71543227170823));
#21896=CARTESIAN_POINT('Ctrl Pts',(91.7711811368466,-0.564680806581021,
1.68430357844077));
#21897=CARTESIAN_POINT('Ctrl Pts',(91.7730336688769,-0.589327924888796,
1.67583880403174));
#21898=CARTESIAN_POINT('Ctrl Pts',(91.7761857451629,-0.631455511862717,
1.66032609492333));
#21899=CARTESIAN_POINT('Ctrl Pts',(91.7774960292812,-0.649026185341669,
1.6535367811025));
#21900=CARTESIAN_POINT('Ctrl Pts',(91.7794088922743,-0.67480995125309,1.64309957896986));
#21901=CARTESIAN_POINT('Ctrl Pts',(91.7800229854057,-0.683108070206707,
1.63966706069126));
#21902=CARTESIAN_POINT('Ctrl Pts',(91.781115959176,-0.697920583288976,1.63340789127914));
#21903=CARTESIAN_POINT('Ctrl Pts',(91.7815961760271,-0.704444442446769,
1.63060495283948));
#21904=CARTESIAN_POINT('Ctrl Pts',(91.7826701311017,-0.71906945257132,1.62421724340548));
#21905=CARTESIAN_POINT('Ctrl Pts',(91.7832625674971,-0.727160784982456,
1.62061091337473));
#21906=CARTESIAN_POINT('Ctrl Pts',(91.7850614349111,-0.751787841983871,
1.60941298249954));
#21907=CARTESIAN_POINT('Ctrl Pts',(91.7862568425081,-0.768234770260599,
1.60162745620269));
#21908=CARTESIAN_POINT('Ctrl Pts',(91.7928718788215,-0.85948670054037,1.55670209981919));
#21909=CARTESIAN_POINT('Ctrl Pts',(91.7980455689796,-0.931727763273796,
1.51457104335979));
#21910=CARTESIAN_POINT('Ctrl Pts',(91.8090871906988,-1.08002453651872,1.41344251073098));
#21911=CARTESIAN_POINT('Ctrl Pts',(91.8149303404641,-1.15479137072698,1.35304422457224));
#21912=CARTESIAN_POINT('Ctrl Pts',(91.8232407852767,-1.25062076575433,1.26187570758489));
#21913=CARTESIAN_POINT('Ctrl Pts',(91.8255455094886,-1.27615377857022,1.23604768741076));
#21914=CARTESIAN_POINT('Ctrl Pts',(91.8296955439495,-1.32007299345992,1.18880873207118));
#21915=CARTESIAN_POINT('Ctrl Pts',(91.8315277288333,-1.3387745237276,1.16770781532602));
#21916=CARTESIAN_POINT('Ctrl Pts',(91.8343652962756,-1.36663234318274,1.13472663854121));
#21917=CARTESIAN_POINT('Ctrl Pts',(91.835355689996,-1.37615405910815,1.12316004567167));
#21918=CARTESIAN_POINT('Ctrl Pts',(91.8371056542482,-1.39261866699155,1.1026358025135));
#21919=CARTESIAN_POINT('Ctrl Pts',(91.8378626406892,-1.39962435619276,1.09372945280813));
#21920=CARTESIAN_POINT('Ctrl Pts',(91.8396026069154,-1.41545847003973,1.07319823325502));
#21921=CARTESIAN_POINT('Ctrl Pts',(91.8405877751235,-1.42422966928899,1.06153047774835));
#21922=CARTESIAN_POINT('Ctrl Pts',(91.8433141545825,-1.44796558775933,1.02913233786918));
#21923=CARTESIAN_POINT('Ctrl Pts',(91.8450667949396,-1.46262756000237,1.00818560506822));
#21924=CARTESIAN_POINT('Ctrl Pts',(91.8561829171046,-1.55186571776381,0.874650648695101));
#21925=CARTESIAN_POINT('Ctrl Pts',(91.8660105609902,-1.61383773358196,0.754198806567161));
#21926=CARTESIAN_POINT('Ctrl Pts',(91.8804739315429,-1.68375778544943,0.569180732782464));
#21927=CARTESIAN_POINT('Ctrl Pts',(91.8850566363689,-1.70282642520583,0.509303449289825));
#21928=CARTESIAN_POINT('Ctrl Pts',(91.8919989415696,-1.72735703059993,0.415308602374065));
#21929=CARTESIAN_POINT('Ctrl Pts',(91.8944232036531,-1.7350645956287,0.381830802954414));
#21930=CARTESIAN_POINT('Ctrl Pts',(91.8975800912173,-1.74400306373291,0.337111335901463));
#21931=CARTESIAN_POINT('Ctrl Pts',(91.8983541432809,-1.74610419988145,0.326053490808516));
#21932=CARTESIAN_POINT('Ctrl Pts',(91.8996286390645,-1.74941483822113,0.307679626733279));
#21933=CARTESIAN_POINT('Ctrl Pts',(91.9001322838279,-1.75068386999912,0.300374804640621));
#21934=CARTESIAN_POINT('Ctrl Pts',(91.9011520465193,-1.75317380398139,0.285490128164897));
#21935=CARTESIAN_POINT('Ctrl Pts',(91.9016679795735,-1.75439136861259,0.277909934368844));
#21936=CARTESIAN_POINT('Ctrl Pts',(91.9030162476974,-1.75746042734692,0.257978452724952));
#21937=CARTESIAN_POINT('Ctrl Pts',(91.9038441972181,-1.75923091042241,0.245614864237416));
#21938=CARTESIAN_POINT('Ctrl Pts',(91.9075057845089,-1.76653874757136,0.190441939138185));
#21939=CARTESIAN_POINT('Ctrl Pts',(91.9102700285676,-1.77064540358375,0.147454389309093));
#21940=CARTESIAN_POINT('Ctrl Pts',(91.9190531877026,-1.77883314519859,0.00833144120753962));
#21941=CARTESIAN_POINT('Ctrl Pts',(91.924891945633,-1.7766752984376,-0.0879991154976709));
#21942=CARTESIAN_POINT('Ctrl Pts',(91.9363074492755,-1.75749720032711,-0.27245798831861));
#21943=CARTESIAN_POINT('Ctrl Pts',(91.9418567939805,-1.74159120012447,-0.360398758734652));
#21944=CARTESIAN_POINT('Ctrl Pts',(91.9493150138125,-1.712498448419,-0.472347009752864));
#21945=CARTESIAN_POINT('Ctrl Pts',(91.951035518596,-1.70528076420434,-0.497775080151869));
#21946=CARTESIAN_POINT('Ctrl Pts',(91.9537365372346,-1.69319176047877,-0.537009932927673));
#21947=CARTESIAN_POINT('Ctrl Pts',(91.9547042931065,-1.68871239387534,-0.550934147674725));
#21948=CARTESIAN_POINT('Ctrl Pts',(91.9565155219082,-1.68005889553645,-0.576736194935529));
#21949=CARTESIAN_POINT('Ctrl Pts',(91.9573574721371,-1.67592943177664,-0.588628114043661));
#21950=CARTESIAN_POINT('Ctrl Pts',(91.9592466105132,-1.66642890397615,-0.615076823189348));
#21951=CARTESIAN_POINT('Ctrl Pts',(91.9602959108043,-1.66099285731871,-0.629608999047637));
#21952=CARTESIAN_POINT('Ctrl Pts',(91.962996250949,-1.64660315834898,-0.666593056353544));
#21953=CARTESIAN_POINT('Ctrl Pts',(91.9646561435933,-1.63738057228142,-0.688936154787929));
#21954=CARTESIAN_POINT('Ctrl Pts',(91.9749417825677,-1.57795956540621,-0.824953840683884));
#21955=CARTESIAN_POINT('Ctrl Pts',(91.9839533423938,-1.51641022468229,-0.933271170475915));
#21956=CARTESIAN_POINT('Ctrl Pts',(91.9981093751224,-1.40370587949371,-1.09063357379551));
#21957=CARTESIAN_POINT('Ctrl Pts',(92.0031834121047,-1.36006431738604,-1.14459502019992));
#21958=CARTESIAN_POINT('Ctrl Pts',(92.0107548787148,-1.28886123290988,-1.2227946855183));
#21959=CARTESIAN_POINT('Ctrl Pts',(92.0133294203464,-1.26352033314355,-1.24896233599829));
#21960=CARTESIAN_POINT('Ctrl Pts',(92.0166473109977,-1.22915310485126,-1.28233324486217));
#21961=CARTESIAN_POINT('Ctrl Pts',(92.0174373557782,-1.22083770706403,-1.29025238485724));
#21962=CARTESIAN_POINT('Ctrl Pts',(92.0187309907237,-1.2069935217153,-1.30318316555679));
#21963=CARTESIAN_POINT('Ctrl Pts',(92.0192379727642,-1.20150902865715,-1.30824148573596));
#21964=CARTESIAN_POINT('Ctrl Pts',(92.0202571770162,-1.19036055803366,-1.31839441494967));
#21965=CARTESIAN_POINT('Ctrl Pts',(92.0207692855079,-1.18469538008056,-1.32348742095573));
#21966=CARTESIAN_POINT('Ctrl Pts',(92.0220957296958,-1.16986143648105,-1.33665159378802));
#21967=CARTESIAN_POINT('Ctrl Pts',(92.0229059355096,-1.16064169083018,-1.34466506977725));
#21968=CARTESIAN_POINT('Ctrl Pts',(92.0263493872838,-1.12081272729846,-1.3785681014705));
#21969=CARTESIAN_POINT('Ctrl Pts',(92.0289231063123,-1.08941216027471,-1.40351447086431));
#21970=CARTESIAN_POINT('Ctrl Pts',(92.0376764168079,-0.978115845369659,
-1.48594636884029));
#21971=CARTESIAN_POINT('Ctrl Pts',(92.0436487359532,-0.894304958489487,
-1.53784538128026));
#21972=CARTESIAN_POINT('Ctrl Pts',(92.0552677409654,-0.726079608906529,
-1.62359010624519));
#21973=CARTESIAN_POINT('Ctrl Pts',(92.0608847387086,-0.642529731144645,
-1.65842977746595));
#21974=CARTESIAN_POINT('Ctrl Pts',(92.0684253573349,-0.531456170209446,
-1.69508846539179));
#21975=CARTESIAN_POINT('Ctrl Pts',(92.0701553536954,-0.506032545487175,
-1.70285099438323));
#21976=CARTESIAN_POINT('Ctrl Pts',(92.0728680004031,-0.46633431263439,-1.71400443727344));
#21977=CARTESIAN_POINT('Ctrl Pts',(92.0738377098263,-0.452175098528091,
-1.71779409731215));
#21978=CARTESIAN_POINT('Ctrl Pts',(92.0756507426971,-0.425772961978432,
-1.72451148735308));
#21979=CARTESIAN_POINT('Ctrl Pts',(92.0764925185536,-0.413542605697971,
-1.72748516183582));
#21980=CARTESIAN_POINT('Ctrl Pts',(92.0783788574649,-0.386204729737495,
-1.73382511161694));
#21981=CARTESIAN_POINT('Ctrl Pts',(92.0794255028663,-0.371082889453845,
-1.73712436906814));
#21982=CARTESIAN_POINT('Ctrl Pts',(92.0825036208095,-0.326759572922621,
-1.74618961199936));
#21983=CARTESIAN_POINT('Ctrl Pts',(92.0845518293549,-0.297455208408674,
-1.7514194793164));
#21984=CARTESIAN_POINT('Ctrl Pts',(92.0962935114343,-0.130610694939501,
-1.77688782294627));
#21985=CARTESIAN_POINT('Ctrl Pts',(92.1064653124034,0.00878068179485438,
-1.7816563613688));
#21986=CARTESIAN_POINT('Ctrl Pts',(92.1220276840634,0.221114897287929,-1.76399061123504));
#21987=CARTESIAN_POINT('Ctrl Pts',(92.1274070239509,0.294508989966902,-1.75323164953646));
#21988=CARTESIAN_POINT('Ctrl Pts',(92.1338625866123,0.384588060156227,-1.73420829242975));
#21989=CARTESIAN_POINT('Ctrl Pts',(92.1351102108654,0.402097367072228,-1.73023239677276));
#21990=CARTESIAN_POINT('Ctrl Pts',(92.1369498025625,0.428106734187949,-1.72391018780301));
#21991=CARTESIAN_POINT('Ctrl Pts',(92.1375521031531,0.436653894719554,-1.72176511058206));
#21992=CARTESIAN_POINT('Ctrl Pts',(92.1385853088255,0.451376416154418,-1.71795352001386));
#21993=CARTESIAN_POINT('Ctrl Pts',(92.1390178730658,0.457559112104252,-1.71631717014676));
#21994=CARTESIAN_POINT('Ctrl Pts',(92.1400317631408,0.472095266265816,-1.71238580977867));
#21995=CARTESIAN_POINT('Ctrl Pts',(92.1406114929616,0.480440933777247,-1.71006304532222));
#21996=CARTESIAN_POINT('Ctrl Pts',(92.1423317172581,0.505293853975976,-1.70294967837966));
#21997=CARTESIAN_POINT('Ctrl Pts',(92.1434625455105,0.521749452693285,-1.69798028504208));
#21998=CARTESIAN_POINT('Ctrl Pts',(92.1517290200104,0.642661868524556,-1.65954232393089));
#21999=CARTESIAN_POINT('Ctrl Pts',(92.1584242322625,0.743904502015605,-1.61669649032372));
#22000=CARTESIAN_POINT('Ctrl Pts',(92.1714619427221,0.93101957165145,-1.5161831720467));
#22001=CARTESIAN_POINT('Ctrl Pts',(92.1777779170461,1.01708857960022,-1.45984136232376));
#22002=CARTESIAN_POINT('Ctrl Pts',(92.1863682453358,1.12242973853387,-1.37702459188812));
#22003=CARTESIAN_POINT('Ctrl Pts',(92.1883982760072,1.14653699270516,-1.35701804606764));
#22004=CARTESIAN_POINT('Ctrl Pts',(92.1914766676314,1.18182770762601,-1.32611848874536));
#22005=CARTESIAN_POINT('Ctrl Pts',(92.1925056786124,1.19341785785592,-1.31569782526542));
#22006=CARTESIAN_POINT('Ctrl Pts',(92.1943777408234,1.21412170667499,-1.29658440464684));
#22007=CARTESIAN_POINT('Ctrl Pts',(92.1952185068084,1.22328302614618,-1.28794458766101));
#22008=CARTESIAN_POINT('Ctrl Pts',(92.1970414024861,1.24284646691842,-1.26909774612404));
#22009=CARTESIAN_POINT('Ctrl Pts',(92.1980248960732,1.25321632151024,-1.25885871286726));
#22010=CARTESIAN_POINT('Ctrl Pts',(92.2007419485579,1.28135119760027,-1.23038659398809));
#22011=CARTESIAN_POINT('Ctrl Pts',(92.2024868085714,1.29885147415598,-1.21189801271387));
#22012=CARTESIAN_POINT('Ctrl Pts',(92.2136603939448,1.4072993783695,-1.09227780103013));
#22013=CARTESIAN_POINT('Ctrl Pts',(92.2235610967633,1.48676021584207,-0.981373136811511));
#22014=CARTESIAN_POINT('Ctrl Pts',(92.2380544706016,1.58300710073718,-0.808101152675607));
#22015=CARTESIAN_POINT('Ctrl Pts',(92.2425963608807,1.61035424642723,-0.752129641879309));
#22016=CARTESIAN_POINT('Ctrl Pts',(92.2494858157535,1.64807151500799,-0.663393921046877));
#22017=CARTESIAN_POINT('Ctrl Pts',(92.251897030935,1.66052685562834,-0.631571164964032));
#22018=CARTESIAN_POINT('Ctrl Pts',(92.2550398795592,1.67584856121881,-0.588830943434232));
#22019=CARTESIAN_POINT('Ctrl Pts',(92.2558124950465,1.67953947155165,-0.578219214579228));
#22020=CARTESIAN_POINT('Ctrl Pts',(92.2570852778343,1.68549726151928,-0.560551469105874));
#22021=CARTESIAN_POINT('Ctrl Pts',(92.2575886290755,1.68782107173756,-0.553515135286951));
#22022=CARTESIAN_POINT('Ctrl Pts',(92.2586084750066,1.69246448612714,-0.539154014804802));
#22023=CARTESIAN_POINT('Ctrl Pts',(92.259124778183,1.69478071803537,-0.531828366962221));
#22024=CARTESIAN_POINT('Ctrl Pts',(92.2604751386562,1.70074485226118,-0.51253062267433));
#22025=CARTESIAN_POINT('Ctrl Pts',(92.2613047857374,1.70431395985522,-0.500534354468809));
#22026=CARTESIAN_POINT('Ctrl Pts',(92.2649878024943,1.71971057940575,-0.446709134278103));
#22027=CARTESIAN_POINT('Ctrl Pts',(92.2677707691593,1.73012804537282,-0.404488751248554));
#22028=CARTESIAN_POINT('Ctrl Pts',(92.276556990232,1.75854201205792,-0.267964616486354));
#22029=CARTESIAN_POINT('Ctrl Pts',(92.2823826576816,1.77045114333896,-0.172568675480497));
#22030=CARTESIAN_POINT('Ctrl Pts',(92.2888893700168,1.77501388171394,-0.0669643044145619));
#22031=CARTESIAN_POINT('Ctrl Pts',(92.2894881254696,1.77535361373816,-0.0572537193054558));
#22032=CARTESIAN_POINT('Ctrl Pts',(92.2900876926257,1.77561363877829,-0.0475422789160742));
#22033=CARTESIAN_POINT('Origin',(88.3562164250559,0.,0.));
#22034=CARTESIAN_POINT('',(93.1870734163657,1.77561363809323,-0.0475423045015944));
#22035=CARTESIAN_POINT('',(93.0389806716583,1.77561363838114,-0.0475422937485569));
#22036=CARTESIAN_POINT('',(88.3562164250559,1.77561363837197,-0.0475422940912398));
#22037=CARTESIAN_POINT('Ctrl Pts',(93.1870734170205,1.77561363809212,-0.0475423045429159));
#22038=CARTESIAN_POINT('Ctrl Pts',(93.1843673805862,1.77446631716615,-0.0903925345226306));
#22039=CARTESIAN_POINT('Ctrl Pts',(93.1817066455266,1.77176788935747,-0.133200198010226));
#22040=CARTESIAN_POINT('Ctrl Pts',(93.1704258635094,1.7536542695672,-0.315233559152988));
#22041=CARTESIAN_POINT('Ctrl Pts',(93.1619621166615,1.72335900659772,-0.452444856457427));
#22042=CARTESIAN_POINT('Ctrl Pts',(93.1512695216931,1.66858663503551,-0.609572023947492));
#22043=CARTESIAN_POINT('Ctrl Pts',(93.1495592451614,1.65935381954731,-0.634274544278217));
#22044=CARTESIAN_POINT('Ctrl Pts',(93.1467672866258,1.64355573744733,-0.673833813572958));
#22045=CARTESIAN_POINT('Ctrl Pts',(93.145696890934,1.63733041970008,-0.688822573714308));
#22046=CARTESIAN_POINT('Ctrl Pts',(93.1437724891179,1.625845524013,-0.715439170253147));
#22047=CARTESIAN_POINT('Ctrl Pts',(93.1429211990053,1.62066431823258,-0.727099736830207));
#22048=CARTESIAN_POINT('Ctrl Pts',(93.1411003149421,1.6093718737776,-0.751793471311541));
#22049=CARTESIAN_POINT('Ctrl Pts',(93.1401296066326,1.60322696207297,-0.764810132269781));
#22050=CARTESIAN_POINT('Ctrl Pts',(93.1374671879178,1.58603888844342,-0.800101738619688));
#22051=CARTESIAN_POINT('Ctrl Pts',(93.1357648103294,1.57468553774726,-0.822221074750268));
#22052=CARTESIAN_POINT('Ctrl Pts',(93.1264507071165,1.51064967405584,-0.940785928120775));
#22053=CARTESIAN_POINT('Ctrl Pts',(93.1185425967317,1.44957549047646,-1.03240689354177));
#22054=CARTESIAN_POINT('Ctrl Pts',(93.1022224701107,1.30890587238961,-1.20613088569067));
#22055=CARTESIAN_POINT('Ctrl Pts',(93.0938417551999,1.22904976357941,-1.28741087716945));
#22056=CARTESIAN_POINT('Ctrl Pts',(93.0847061384313,1.12910405227286,-1.37130235895337));
#22057=CARTESIAN_POINT('Ctrl Pts',(93.0835403350365,1.11608728938702,-1.38191726748776));
#22058=CARTESIAN_POINT('Ctrl Pts',(93.0817860293388,1.09606923888548,-1.39777419428674));
#22059=CARTESIAN_POINT('Ctrl Pts',(93.0811888070299,1.08917696967992,-1.40315145708248));
#22060=CARTESIAN_POINT('Ctrl Pts',(93.0801562750995,1.07712076060961,-1.41241519811146));
#22061=CARTESIAN_POINT('Ctrl Pts',(93.0797194060113,1.07197505125258,-1.41632458053809));
#22062=CARTESIAN_POINT('Ctrl Pts',(93.0786838944363,1.05967204171987,-1.42556616033597));
#22063=CARTESIAN_POINT('Ctrl Pts',(93.0780870217076,1.05249575016018,-1.43087260717026));
#22064=CARTESIAN_POINT('Ctrl Pts',(93.0762789259939,1.03050921498149,-1.44687544680128));
#22065=CARTESIAN_POINT('Ctrl Pts',(93.0750787889028,1.01557317178617,-1.45739802294471));
#22066=CARTESIAN_POINT('Ctrl Pts',(93.0689209533595,0.937328876468771,-1.51073466917814));
#22067=CARTESIAN_POINT('Ctrl Pts',(93.0641668884786,0.87146133019501,-1.54966526005496));
#22068=CARTESIAN_POINT('Ctrl Pts',(93.0504766827301,0.673310650565444,-1.65013727612473));
#22069=CARTESIAN_POINT('Ctrl Pts',(93.0416621358394,0.535735953823592,-1.69978921579432));
#22070=CARTESIAN_POINT('Ctrl Pts',(93.0306563655123,0.369707433424003,-1.73752212495236));
#22071=CARTESIAN_POINT('Ctrl Pts',(93.0290552666102,0.345659566130191,-1.74246552034583));
#22072=CARTESIAN_POINT('Ctrl Pts',(93.0264946158224,0.307425470731535,-1.74950249106907));
#22073=CARTESIAN_POINT('Ctrl Pts',(93.0255455505255,0.293302534992512,-1.75192550897179));
#22074=CARTESIAN_POINT('Ctrl Pts',(93.0237402903007,0.266539947072141,-1.75618439111149));
#22075=CARTESIAN_POINT('Ctrl Pts',(93.0228852694801,0.253906737887011,-1.75805532128426));
#22076=CARTESIAN_POINT('Ctrl Pts',(93.0209264008257,0.225067367983645,-1.76200899482881));
#22077=CARTESIAN_POINT('Ctrl Pts',(93.0198198758359,0.20885064657166,-1.76400464688679));
#22078=CARTESIAN_POINT('Ctrl Pts',(93.0163238802699,0.157862238576624,-1.76956641309156));
#22079=CARTESIAN_POINT('Ctrl Pts',(93.0139097300579,0.123013307105346,-1.77232988018401));
#22080=CARTESIAN_POINT('Ctrl Pts',(92.9999928010988,-0.0757404713423424,
-1.78220084245671));
#22081=CARTESIAN_POINT('Ctrl Pts',(92.9878210116381,-0.239911681590536,
-1.76759747852855));
#22082=CARTESIAN_POINT('Ctrl Pts',(92.9723562543569,-0.448349156027029,
-1.71945921412546));
#22083=CARTESIAN_POINT('Ctrl Pts',(92.9687914126519,-0.496507019657609,
-1.70617662834811));
#22084=CARTESIAN_POINT('Ctrl Pts',(92.9644079428029,-0.556535988513159,
-1.6868621532881));
#22085=CARTESIAN_POINT('Ctrl Pts',(92.9635024540357,-0.568982205374252,
-1.68270481853185));
#22086=CARTESIAN_POINT('Ctrl Pts',(92.962066432522,-0.588812232377587,-1.67583592741605));
#22087=CARTESIAN_POINT('Ctrl Pts',(92.9615310675691,-0.596225809967661,
-1.67321268528922));
#22088=CARTESIAN_POINT('Ctrl Pts',(92.9604961718943,-0.610601856938426,
-1.66801814004576));
#22089=CARTESIAN_POINT('Ctrl Pts',(92.9599963686371,-0.617565990660018,
-1.66545230879401));
#22090=CARTESIAN_POINT('Ctrl Pts',(92.9587600187878,-0.634839669341869,
-1.6589648328293));
#22091=CARTESIAN_POINT('Ctrl Pts',(92.9580265155479,-0.645129381522193,
-1.65499057970824));
#22092=CARTESIAN_POINT('Ctrl Pts',(92.9551928964557,-0.685007733688089,
-1.63915968916185));
#22093=CARTESIAN_POINT('Ctrl Pts',(92.9531301053352,-0.714313984906699,
-1.62660256639049));
#22094=CARTESIAN_POINT('Ctrl Pts',(92.9475576639566,-0.793656333575301,
-1.59004765945956));
#22095=CARTESIAN_POINT('Ctrl Pts',(92.9441100354529,-0.842932531552592,
-1.56448314921777));
#22096=CARTESIAN_POINT('Ctrl Pts',(92.9319877639403,-1.01301471285963,-1.46587136257078));
#22097=CARTESIAN_POINT('Ctrl Pts',(92.9234582465617,-1.12621472543064,-1.38080230647322));
#22098=CARTESIAN_POINT('Ctrl Pts',(92.9127366014071,-1.24662940472908,-1.26555645510259));
#22099=CARTESIAN_POINT('Ctrl Pts',(92.9110766451555,-1.26471925088722,-1.2474787071396));
#22100=CARTESIAN_POINT('Ctrl Pts',(92.9083503863304,-1.29348459470841,-1.21746365927781));
#22101=CARTESIAN_POINT('Ctrl Pts',(92.9072944936625,-1.30440038022468,-1.20576107855679));
#22102=CARTESIAN_POINT('Ctrl Pts',(92.9053858656151,-1.32371891678303,-1.18448072047841));
#22103=CARTESIAN_POINT('Ctrl Pts',(92.9045356672638,-1.33217965090295,-1.17495689751596));
#22104=CARTESIAN_POINT('Ctrl Pts',(92.9027058099775,-1.35007601430589,-1.15437005253446));
#22105=CARTESIAN_POINT('Ctrl Pts',(92.9017249119142,-1.35947965580081,-1.14328058941164));
#22106=CARTESIAN_POINT('Ctrl Pts',(92.899003764132,-1.3850389887192,-1.11237789948475));
#22107=CARTESIAN_POINT('Ctrl Pts',(92.897252038892,-1.40090415594431,-1.09233008688981));
#22108=CARTESIAN_POINT('Ctrl Pts',(92.8932809637014,-1.43554363353485,-1.04656204729599));
#22109=CARTESIAN_POINT('Ctrl Pts',(92.8910530477858,-1.45406971606169,-1.02066580627248));
#22110=CARTESIAN_POINT('Ctrl Pts',(92.8834946910346,-1.51390978920111,-0.932081786295268));
#22111=CARTESIAN_POINT('Ctrl Pts',(92.8780635928175,-1.55194097204341,-0.867281115467987));
#22112=CARTESIAN_POINT('Ctrl Pts',(92.8641441341732,-1.63786329875699,-0.697024873027511));
#22113=CARTESIAN_POINT('Ctrl Pts',(92.8556119688851,-1.67976500427924,-0.588925478803648));
#22114=CARTESIAN_POINT('Ctrl Pts',(92.8463537898442,-1.71532586980725,-0.461516056973144));
#22115=CARTESIAN_POINT('Ctrl Pts',(92.8452011798296,-1.71956642934384,-0.445456232595381));
#22116=CARTESIAN_POINT('Ctrl Pts',(92.8434626004822,-1.72568470341,-0.420894399555913));
#22117=CARTESIAN_POINT('Ctrl Pts',(92.84286813445,-1.72772609635524,-0.412434643526438));
#22118=CARTESIAN_POINT('Ctrl Pts',(92.8417939683239,-1.73132371965613,-0.397030078767995));
#22119=CARTESIAN_POINT('Ctrl Pts',(92.8413131744304,-1.73290045498333,-0.390090658967901));
#22120=CARTESIAN_POINT('Ctrl Pts',(92.840207557654,-1.73644787711398,-0.374031907282422));
#22121=CARTESIAN_POINT('Ctrl Pts',(92.839584425486,-1.73838847777447,-0.364906299787943));
#22122=CARTESIAN_POINT('Ctrl Pts',(92.8376070696733,-1.74435383594001,-0.335726249982958));
#22123=CARTESIAN_POINT('Ctrl Pts',(92.8362671627631,-1.74810430606625,-0.315616606699628));
#22124=CARTESIAN_POINT('Ctrl Pts',(92.833058508216,-1.75634162093474,-0.266782875578532));
#22125=CARTESIAN_POINT('Ctrl Pts',(92.8312050931124,-1.76047243829011,-0.238004143461919));
#22126=CARTESIAN_POINT('Ctrl Pts',(92.8234306336066,-1.77498732249631,-0.115582370821546));
#22127=CARTESIAN_POINT('Ctrl Pts',(92.8177068178969,-1.7786197400268,-0.0212896962673536));
#22128=CARTESIAN_POINT('Ctrl Pts',(92.8058156854698,-1.77069192889892,0.171843713879389));
#22129=CARTESIAN_POINT('Ctrl Pts',(92.7996581036799,-1.75835397810964,0.27031081915597));
#22130=CARTESIAN_POINT('Ctrl Pts',(92.7917713932719,-1.73319728442869,0.389362278079672));
#22131=CARTESIAN_POINT('Ctrl Pts',(92.7902928802,-1.7280981413152,0.411403146030047));
#22132=CARTESIAN_POINT('Ctrl Pts',(92.7878824979592,-1.71918224409287,0.44684494451532));
#22133=CARTESIAN_POINT('Ctrl Pts',(92.7869590411346,-1.71562621974485,0.460309296316371));
#22134=CARTESIAN_POINT('Ctrl Pts',(92.7851719168077,-1.70847872115155,0.486138118032187));
#22135=CARTESIAN_POINT('Ctrl Pts',(92.7843090518241,-1.70491039326013,0.498508120566227));
#22136=CARTESIAN_POINT('Ctrl Pts',(92.7822862601781,-1.69627516346444,0.527265423220525));
#22137=CARTESIAN_POINT('Ctrl Pts',(92.7811230124424,-1.69110480648257,0.543620045736141));
#22138=CARTESIAN_POINT('Ctrl Pts',(92.7772324613061,-1.67314329655655,0.59769732372607));
#22139=CARTESIAN_POINT('Ctrl Pts',(92.7744718236204,-1.65932104596304,0.635062052097813));
#22140=CARTESIAN_POINT('Ctrl Pts',(92.767559884455,-1.62211205029763,0.726115082455237));
#22141=CARTESIAN_POINT('Ctrl Pts',(92.7633678110767,-1.59730538737095,0.779169436418959));
#22142=CARTESIAN_POINT('Ctrl Pts',(92.750974053264,-1.51730275344643,0.93032908987476));
#22143=CARTESIAN_POINT('Ctrl Pts',(92.7426514302909,-1.45535271419137,1.02453310607392));
#22144=CARTESIAN_POINT('Ctrl Pts',(92.731876610334,-1.36126411094349,1.14168737692302));
#22145=CARTESIAN_POINT('Ctrl Pts',(92.7292022422055,-1.3366834333077,1.17037084376798));
#22146=CARTESIAN_POINT('Ctrl Pts',(92.7257470983207,-1.30307395845825,1.20714854199916));
#22147=CARTESIAN_POINT('Ctrl Pts',(92.7249169123541,-1.2948522360585,1.21596342486316));
#22148=CARTESIAN_POINT('Ctrl Pts',(92.7236232396188,-1.28179969613591,1.22967511643292));
#22149=CARTESIAN_POINT('Ctrl Pts',(92.7231554120005,-1.27702926548414,1.23462853205417));
#22150=CARTESIAN_POINT('Ctrl Pts',(92.722186917708,-1.26704604054714,1.24487492456682));
#22151=CARTESIAN_POINT('Ctrl Pts',(92.7216866732231,-1.26182862575356,1.25016309674087));
#22152=CARTESIAN_POINT('Ctrl Pts',(92.7204475024709,-1.24875676082029,1.26324703639823));
#22153=CARTESIAN_POINT('Ctrl Pts',(92.7197116506484,-1.24086217068869,1.27100260096203));
#22154=CARTESIAN_POINT('Ctrl Pts',(92.7168564198474,-1.20973659536803,1.30101359179794));
#22155=CARTESIAN_POINT('Ctrl Pts',(92.7147750960966,-1.18597374780656,1.32271144603613));
#22156=CARTESIAN_POINT('Ctrl Pts',(92.7091334567072,-1.11904254874655,1.38057138322055));
#22157=CARTESIAN_POINT('Ctrl Pts',(92.7056370449854,-1.07472279400941,1.41534637248659));
#22158=CARTESIAN_POINT('Ctrl Pts',(92.6931103558333,-0.909051133620568,
1.53306159289965));
#22159=CARTESIAN_POINT('Ctrl Pts',(92.6842278957725,-0.779196297777744,
1.6029663470421));
#22160=CARTESIAN_POINT('Ctrl Pts',(92.6731531225254,-0.619495007711486,
1.66489762911858));
#22161=CARTESIAN_POINT('Ctrl Pts',(92.671563117473,-0.596591405779294,1.67324139942057));
#22162=CARTESIAN_POINT('Ctrl Pts',(92.6690160703683,-0.559997049039636,
1.68572585254875));
#22163=CARTESIAN_POINT('Ctrl Pts',(92.66806931944,-0.546414991197009,1.69017720435915));
#22164=CARTESIAN_POINT('Ctrl Pts',(92.6662658730183,-0.520591620046023,
1.69829670503486));
#22165=CARTESIAN_POINT('Ctrl Pts',(92.6654103194738,-0.50836150123457,1.70199762118008));
#22166=CARTESIAN_POINT('Ctrl Pts',(92.6634465523734,-0.480343410667287,
1.71014715698984));
#22167=CARTESIAN_POINT('Ctrl Pts',(92.6623356119028,-0.464531816512941,
1.71450962395588));
#22168=CARTESIAN_POINT('Ctrl Pts',(92.6588101012366,-0.414492088314664,
1.72757273741767));
#22169=CARTESIAN_POINT('Ctrl Pts',(92.6563702505991,-0.380065498998132,
1.73547145261305));
#22170=CARTESIAN_POINT('Ctrl Pts',(92.6504547129736,-0.297124696358117,
1.7519149336425));
#22171=CARTESIAN_POINT('Ctrl Pts',(92.6469522730853,-0.248447506173411,
1.75947780508053));
#22172=CARTESIAN_POINT('Ctrl Pts',(92.6381958553743,-0.127592410754624,
1.77313966993264));
#22173=CARTESIAN_POINT('Ctrl Pts',(92.632898490908,-0.0552358435429476,
1.77686580972084));
#22174=CARTESIAN_POINT('Ctrl Pts',(92.6215499092297,0.0999696476038994,
1.77536790231446));
#22175=CARTESIAN_POINT('Ctrl Pts',(92.6155130170895,0.18264790660041,1.76877568174811));
#22176=CARTESIAN_POINT('Ctrl Pts',(92.608420214926,0.282625809337143,1.75371608313486));
#22177=CARTESIAN_POINT('Ctrl Pts',(92.607150862131,0.30063887253928,1.75071807597795));
#22178=CARTESIAN_POINT('Ctrl Pts',(92.6052822199219,0.327381534363827,1.74584220691877));
#22179=CARTESIAN_POINT('Ctrl Pts',(92.6046722337553,0.336147769607939,1.74417555484587));
#22180=CARTESIAN_POINT('Ctrl Pts',(92.6035785016835,0.351938807013144,1.74104985726787));
#22181=CARTESIAN_POINT('Ctrl Pts',(92.6030935195458,0.358967683711983,1.73961424913318));
#22182=CARTESIAN_POINT('Ctrl Pts',(92.6019980814948,0.374904017415935,1.73625863816039));
#22183=CARTESIAN_POINT('Ctrl Pts',(92.6013890902225,0.383805615585702,1.73431264176113));
#22184=CARTESIAN_POINT('Ctrl Pts',(92.5995041225156,0.411473383485588,1.728040676784));
#22185=CARTESIAN_POINT('Ctrl Pts',(92.59824064781,0.430185140408706,1.72347780514776));
#22186=CARTESIAN_POINT('Ctrl Pts',(92.5952516530929,0.474733492895714,1.71184388456262));
#22187=CARTESIAN_POINT('Ctrl Pts',(92.5935388206373,0.500492098181849,1.70449088744428));
#22188=CARTESIAN_POINT('Ctrl Pts',(92.5867771191196,0.60257091033138,1.67283785455456));
#22189=CARTESIAN_POINT('Ctrl Pts',(92.5818774607109,0.677379250394012,1.6439699592017));
#22190=CARTESIAN_POINT('Ctrl Pts',(92.5703049807169,0.848278740652362,1.56436709076239));
#22191=CARTESIAN_POINT('Ctrl Pts',(92.5636321382201,0.942160198277295,1.50968601847097));
#22192=CARTESIAN_POINT('Ctrl Pts',(92.5550542281034,1.05066392282222,1.4324050772597));
#22193=CARTESIAN_POINT('Ctrl Pts',(92.5534432425005,1.07055775764301,1.4175983122861));
#22194=CARTESIAN_POINT('Ctrl Pts',(92.5507810355504,1.10259289434307,1.39269593874321));
#22195=CARTESIAN_POINT('Ctrl Pts',(92.5497394018812,1.11492146358133,1.38284604048533));
#22196=CARTESIAN_POINT('Ctrl Pts',(92.5478460131526,1.1369499735396,1.36476030364418));
#22197=CARTESIAN_POINT('Ctrl Pts',(92.5469966190884,1.14669585758813,1.35658192691669));
#22198=CARTESIAN_POINT('Ctrl Pts',(92.5451566192781,1.16750963280789,1.33873124640728));
#22199=CARTESIAN_POINT('Ctrl Pts',(92.5441646414813,1.17854693641908,1.32902490149817));
#22200=CARTESIAN_POINT('Ctrl Pts',(92.5413791568657,1.20902086816311,1.30154759760218));
#22201=CARTESIAN_POINT('Ctrl Pts',(92.5395732593836,1.22818391416243,1.28348032780835));
#22202=CARTESIAN_POINT('Ctrl Pts',(92.5354571556932,1.27051252708568,1.24175593492237));
#22203=CARTESIAN_POINT('Ctrl Pts',(92.5331374083657,1.29343204777661,1.21786418815922));
#22204=CARTESIAN_POINT('Ctrl Pts',(92.525099372151,1.3696864335583,1.13379346799066));
#22205=CARTESIAN_POINT('Ctrl Pts',(92.5192656699838,1.41959244019577,1.07064632140312));
#22206=CARTESIAN_POINT('Ctrl Pts',(92.5056019401028,1.52531764912201,0.916423788946797));
#22207=CARTESIAN_POINT('Ctrl Pts',(92.4977626504106,1.57755751704793,0.823251111969195));
#22208=CARTESIAN_POINT('Ctrl Pts',(92.4890677419122,1.628274704619,0.70999380186209));
#22209=CARTESIAN_POINT('Ctrl Pts',(92.4878535218679,1.6351842881486,0.693932355238349));
#22210=CARTESIAN_POINT('Ctrl Pts',(92.4860495985289,1.64520316973356,0.669662261787435));
#22211=CARTESIAN_POINT('Ctrl Pts',(92.4854502077736,1.64849040222139,0.661528847880037));
#22212=CARTESIAN_POINT('Ctrl Pts',(92.4844156025092,1.65409383589656,0.647363410960038));
#22213=CARTESIAN_POINT('Ctrl Pts',(92.4839788023657,1.65643751288348,0.641342788977989));
#22214=CARTESIAN_POINT('Ctrl Pts',(92.4829455458842,1.66192861107751,0.627005910901365));
#22215=CARTESIAN_POINT('Ctrl Pts',(92.4823508328376,1.6650465042067,0.618678646731392));
#22216=CARTESIAN_POINT('Ctrl Pts',(92.48055622859,1.67431949013696,0.593334434793887));
#22217=CARTESIAN_POINT('Ctrl Pts',(92.4793671835334,1.6802774133147,0.576245939692672));
#22218=CARTESIAN_POINT('Ctrl Pts',(92.4733266640321,1.70950532720676,0.488103826572759));
#22219=CARTESIAN_POINT('Ctrl Pts',(92.4686703251204,1.72853596845471,0.415715877133255));
#22220=CARTESIAN_POINT('Ctrl Pts',(92.4559937631666,1.76816132444284,0.213970194009545));
#22221=CARTESIAN_POINT('Ctrl Pts',(92.4480789421171,1.77911485287178,0.0832213624709728));
#22222=CARTESIAN_POINT('Ctrl Pts',(92.4397243119761,1.77561363837196,-0.0475422940915189));
#22223=CARTESIAN_POINT('Ctrl Pts',(92.2900876926257,1.77561363877829,-0.0475422789160742));
#22224=CARTESIAN_POINT('Ctrl Pts',(92.294987767018,1.77773874190886,0.0318262786811712));
#22225=CARTESIAN_POINT('Ctrl Pts',(92.299947488628,1.77454014362674,0.111251623550904));
#22226=CARTESIAN_POINT('Ctrl Pts',(92.3067711489427,1.76320843930912,0.216466768547959));
#22227=CARTESIAN_POINT('Ctrl Pts',(92.3084907290523,1.7597943916703,0.242663230208114));
#22228=CARTESIAN_POINT('Ctrl Pts',(92.3111906212778,1.75358480229037,0.283228286872694));
#22229=CARTESIAN_POINT('Ctrl Pts',(92.3121581933839,1.75119361238491,0.297655558908998));
#22230=CARTESIAN_POINT('Ctrl Pts',(92.3139692636738,1.74641302368818,0.324444278856811));
#22231=CARTESIAN_POINT('Ctrl Pts',(92.3148112416232,1.74406979714128,0.336813105455989));
#22232=CARTESIAN_POINT('Ctrl Pts',(92.3167006846593,1.7385447089143,0.364372350954233));
#22233=CARTESIAN_POINT('Ctrl Pts',(92.3177502649206,1.7352948641781,0.379547918824588));
#22234=CARTESIAN_POINT('Ctrl Pts',(92.3204518236959,1.72647309803166,0.418257766624543));
#22235=CARTESIAN_POINT('Ctrl Pts',(92.3221126684961,1.72061877619451,0.441723719542048));
#22236=CARTESIAN_POINT('Ctrl Pts',(92.3323813330598,1.68182116594911,0.584737500728853));
#22237=CARTESIAN_POINT('Ctrl Pts',(92.341373129795,1.6369176302476,0.700664633085665));
#22238=CARTESIAN_POINT('Ctrl Pts',(92.3555224661115,1.54858882841298,0.872793298223924));
#22239=CARTESIAN_POINT('Ctrl Pts',(92.3606093291823,1.51325037135594,0.93272168129298));
#22240=CARTESIAN_POINT('Ctrl Pts',(92.3681970566756,1.45415533801439,1.02069885504964));
#22241=CARTESIAN_POINT('Ctrl Pts',(92.370775363499,1.43289246135653,1.05033971835392));
#22242=CARTESIAN_POINT('Ctrl Pts',(92.3740972761119,1.40374997655233,1.08843099795434));
#22243=CARTESIAN_POINT('Ctrl Pts',(92.3748877127732,1.39668098175866,1.09748726041403));
#22244=CARTESIAN_POINT('Ctrl Pts',(92.3761818207207,1.38487616689209,1.11231189188534));
#22245=CARTESIAN_POINT('Ctrl Pts',(92.3766888885216,1.38019107500477,1.11812000492222));
#22246=CARTESIAN_POINT('Ctrl Pts',(92.3777080885485,1.3706502669106,1.12979640484841));
#22247=CARTESIAN_POINT('Ctrl Pts',(92.3782201087548,1.36579315343773,1.13566330315372));
#22248=CARTESIAN_POINT('Ctrl Pts',(92.379546052183,1.35305259198395,1.15085263767614));
#22249=CARTESIAN_POINT('Ctrl Pts',(92.380355851296,1.34511034838335,1.16012554561715));
#22250=CARTESIAN_POINT('Ctrl Pts',(92.3837945206381,1.31072632040991,1.19944250077928));
#22251=CARTESIAN_POINT('Ctrl Pts',(92.3863640710019,1.28336683753283,1.22867241459741));
#22252=CARTESIAN_POINT('Ctrl Pts',(92.3951167659577,1.18537199644857,1.32651800615146));
#22253=CARTESIAN_POINT('Ctrl Pts',(92.4010920226929,1.11003594067722,1.39017249541882));
#22254=CARTESIAN_POINT('Ctrl Pts',(92.4127154989047,0.956130603278522,1.49968505749523));
#22255=CARTESIAN_POINT('Ctrl Pts',(92.4183339807237,0.878564988483435,1.546402894642));
#22256=CARTESIAN_POINT('Ctrl Pts',(92.4258764036786,0.774034383404318,1.59895012751027));
#22257=CARTESIAN_POINT('Ctrl Pts',(92.427606603258,0.750019233320723,1.61035454679107));
#22258=CARTESIAN_POINT('Ctrl Pts',(92.4303194958729,0.71237955984429,1.62720443789726));
#22259=CARTESIAN_POINT('Ctrl Pts',(92.4312892439641,0.698927649773842,1.63302756827052));
#22260=CARTESIAN_POINT('Ctrl Pts',(92.4331023078376,0.673793838062607,1.64354018701132));
#22261=CARTESIAN_POINT('Ctrl Pts',(92.4339440754815,0.662131103875427,1.648273299468));
#22262=CARTESIAN_POINT('Ctrl Pts',(92.4358303421586,0.636017786835537,1.65854905173632));
#22263=CARTESIAN_POINT('Ctrl Pts',(92.4368769228631,0.621543228706961,1.66402751496197));
#22264=CARTESIAN_POINT('Ctrl Pts',(92.4399546736348,0.579030950873135,1.6794858966941));
#22265=CARTESIAN_POINT('Ctrl Pts',(92.442002573838,0.550812983393234,1.68895073659823));
#22266=CARTESIAN_POINT('Ctrl Pts',(92.4537443151974,0.389497776793513,1.73858639498199));
#22267=CARTESIAN_POINT('Ctrl Pts',(92.4639165523496,0.252302620802843,1.76372377578804));
#22268=CARTESIAN_POINT('Ctrl Pts',(92.4794795389711,0.039662934929671,1.77735248070115));
#22269=CARTESIAN_POINT('Ctrl Pts',(92.4848590421069,-0.0345176048229986,
1.77746043892314));
#22270=CARTESIAN_POINT('Ctrl Pts',(92.4913147708779,-0.126413895956299,
1.7718368748879));
#22271=CARTESIAN_POINT('Ctrl Pts',(92.492562408806,-0.144316917094056,1.77046860284157));
#22272=CARTESIAN_POINT('Ctrl Pts',(92.4944020140745,-0.170972001694435,
1.7680244020173));
#22273=CARTESIAN_POINT('Ctrl Pts',(92.4950043149143,-0.179741181007259,
1.76715444363687));
#22274=CARTESIAN_POINT('Ctrl Pts',(92.4960375191919,-0.194863196684076,
1.76554051220674));
#22275=CARTESIAN_POINT('Ctrl Pts',(92.4964700818116,-0.201218870654983,
1.76482745201306));
#22276=CARTESIAN_POINT('Ctrl Pts',(92.4974839651924,-0.216173994872004,
1.76306775382044));
#22277=CARTESIAN_POINT('Ctrl Pts',(92.4980636899817,-0.224769803930325,
1.76199252090491));
#22278=CARTESIAN_POINT('Ctrl Pts',(92.4997838856737,-0.250396181731585,
1.75859637943415));
#22279=CARTESIAN_POINT('Ctrl Pts',(92.5009146908052,-0.267401844096548,
1.75609105150427));
#22280=CARTESIAN_POINT('Ctrl Pts',(92.5108680132218,-0.41819640648147,1.73163409889619));
#22281=CARTESIAN_POINT('Ctrl Pts',(92.5190167665743,-0.549117660468979,
1.69467556524703));
#22282=CARTESIAN_POINT('Ctrl Pts',(92.5326543502629,-0.753853549758228,
1.61062526329925));
#22283=CARTESIAN_POINT('Ctrl Pts',(92.5379944662434,-0.830666872730658,
1.57238642009697));
#22284=CARTESIAN_POINT('Ctrl Pts',(92.5451978271474,-0.926757637741552,
1.51553891879538));
#22285=CARTESIAN_POINT('Ctrl Pts',(92.5468884230646,-0.948806235862827,
1.5018337284582));
#22286=CARTESIAN_POINT('Ctrl Pts',(92.549552822635,-0.982715364505309,1.47971136067804));
#22287=CARTESIAN_POINT('Ctrl Pts',(92.5505144382567,-0.994786819273702,
1.4716230365302));
#22288=CARTESIAN_POINT('Ctrl Pts',(92.5523201423367,-1.01713498364249,1.45624831438887));
#22289=CARTESIAN_POINT('Ctrl Pts',(92.553162787542,-1.02743610358784,1.44899888441667));
#22290=CARTESIAN_POINT('Ctrl Pts',(92.5550613655639,-1.05035455017567,1.43250272590971));
#22291=CARTESIAN_POINT('Ctrl Pts',(92.5561195090194,-1.06292844601215,1.42319774877682));
#22292=CARTESIAN_POINT('Ctrl Pts',(92.5588589737818,-1.09496184097549,1.3988309774537));
#22293=CARTESIAN_POINT('Ctrl Pts',(92.5605495922196,-1.114233639748,1.38352912050741));
#22294=CARTESIAN_POINT('Ctrl Pts',(92.5695486355707,-1.21417802700063,1.30073021477178));
#22295=CARTESIAN_POINT('Ctrl Pts',(92.5771231498474,-1.28904252983136,1.22657664855662));
#22296=CARTESIAN_POINT('Ctrl Pts',(92.590856537093,-1.4104386529885,1.08287129223297));
#22297=CARTESIAN_POINT('Ctrl Pts',(92.5969552881937,-1.45947342815113,1.01581768266667));
#22298=CARTESIAN_POINT('Ctrl Pts',(92.6048679601578,-1.51813545058003,0.922534536726264));
#22299=CARTESIAN_POINT('Ctrl Pts',(92.6068060973843,-1.53209719543812,0.899157138910064));
#22300=CARTESIAN_POINT('Ctrl Pts',(92.6100869176921,-1.55510630912288,0.858537701871372));
#22301=CARTESIAN_POINT('Ctrl Pts',(92.611441460623,-1.56441760704115,0.841451273979836));
#22302=CARTESIAN_POINT('Ctrl Pts',(92.6134057981759,-1.57766683504726,0.816158154560689));
#22303=CARTESIAN_POINT('Ctrl Pts',(92.6140279762,-1.58182512234663,0.808069345461167));
#22304=CARTESIAN_POINT('Ctrl Pts',(92.6151292551768,-1.58912011308265,0.793606818001506));
#22305=CARTESIAN_POINT('Ctrl Pts',(92.6156097883214,-1.5922809282663,0.787245810496631));
#22306=CARTESIAN_POINT('Ctrl Pts',(92.6166770728118,-1.59925120226717,0.773004691110172));
#22307=CARTESIAN_POINT('Ctrl Pts',(92.6172626116304,-1.60304067078751,0.765115204609341));
#22308=CARTESIAN_POINT('Ctrl Pts',(92.6190185484187,-1.61429341002019,0.741236921853471));
#22309=CARTESIAN_POINT('Ctrl Pts',(92.6201786745559,-1.62157716251552,0.725164086171876));
#22310=CARTESIAN_POINT('Ctrl Pts',(92.628165516429,-1.67054628389508,0.6126762952755));
#22311=CARTESIAN_POINT('Ctrl Pts',(92.6345925656338,-1.70385228643998,0.512825763812056));
#22312=CARTESIAN_POINT('Ctrl Pts',(92.6433779569992,-1.73693987947621,0.373568125331418));
#22313=CARTESIAN_POINT('Ctrl Pts',(92.6457139748372,-1.74454694920296,0.336257590118528));
#22314=CARTESIAN_POINT('Ctrl Pts',(92.6533469979423,-1.76532886207983,0.214449147564586));
#22315=CARTESIAN_POINT('Ctrl Pts',(92.6587024785329,-1.77360275802386,0.12924798597122));
#22316=CARTESIAN_POINT('Ctrl Pts',(92.6656531572998,-1.77624256056255,0.0221993833918785));
#22317=CARTESIAN_POINT('Ctrl Pts',(92.6670662336691,-1.77638115751821,0.000602915287913788));
#22318=CARTESIAN_POINT('Ctrl Pts',(92.669390537153,-1.77596501978015,-0.0346097630793831));
#22319=CARTESIAN_POINT('Ctrl Pts',(92.6702943196776,-1.77564741253603,-0.0482269221148783));
#22320=CARTESIAN_POINT('Ctrl Pts',(92.6720576206877,-1.77472730201001,-0.0746400551884794));
#22321=CARTESIAN_POINT('Ctrl Pts',(92.6729165164434,-1.77414291769145,-0.0874358453206651));
#22322=CARTESIAN_POINT('Ctrl Pts',(92.6749522437852,-1.77243864758607,-0.117592192289331));
#22323=CARTESIAN_POINT('Ctrl Pts',(92.6761326622277,-1.77120202490211,-0.134944553389764));
#22324=CARTESIAN_POINT('Ctrl Pts',(92.6801952224641,-1.76610420083517,-0.194190318495858));
#22325=CARTESIAN_POINT('Ctrl Pts',(92.6831151845539,-1.76100995122983,-0.235960517560864));
#22326=CARTESIAN_POINT('Ctrl Pts',(92.6905601174575,-1.74449057140451,-0.340398112601972));
#22327=CARTESIAN_POINT('Ctrl Pts',(92.6951351088823,-1.73116943320391,-0.402702447277033));
#22328=CARTESIAN_POINT('Ctrl Pts',(92.7093429924894,-1.68007805351679,-0.591429151290706));
#22329=CARTESIAN_POINT('Ctrl Pts',(92.7191300311273,-1.63155662081395,-0.714476312882583));
#22330=CARTESIAN_POINT('Ctrl Pts',(92.7296305824709,-1.56148809716388,-0.846840782449819));
#22331=CARTESIAN_POINT('Ctrl Pts',(92.7308742653879,-1.55287563305321,-0.862532154787655));
#22332=CARTESIAN_POINT('Ctrl Pts',(92.7327092329734,-1.53967621480268,-0.885741878761088));
#22333=CARTESIAN_POINT('Ctrl Pts',(92.7333107784125,-1.53526845182023,-0.893360124116083));
#22334=CARTESIAN_POINT('Ctrl Pts',(92.7343911775643,-1.52720215624251,-0.907065635334838));
#22335=CARTESIAN_POINT('Ctrl Pts',(92.7348712175243,-1.52356357968976,-0.91316401353071));
#22336=CARTESIAN_POINT('Ctrl Pts',(92.7359569472055,-1.51520995869963,-0.926976032569233));
#22337=CARTESIAN_POINT('Ctrl Pts',(92.7365611836071,-1.51047249462615,-0.934675684788626));
#22338=CARTESIAN_POINT('Ctrl Pts',(92.7384350523057,-1.49551151705059,-0.958580446001442));
#22339=CARTESIAN_POINT('Ctrl Pts',(92.7396922838651,-1.48508407808564,-0.974657130993974));
#22340=CARTESIAN_POINT('Ctrl Pts',(92.7426677880055,-1.45952791938442,-1.01269606499421));
#22341=CARTESIAN_POINT('Ctrl Pts',(92.7443734474866,-1.44416050480417,-1.03449294518712));
#22342=CARTESIAN_POINT('Ctrl Pts',(92.7511068065287,-1.38090725388352,-1.12005213439666));
#22343=CARTESIAN_POINT('Ctrl Pts',(92.7559860196006,-1.32924063079203,-1.18090755502804));
#22344=CARTESIAN_POINT('Ctrl Pts',(92.767601040113,-1.1973454107804,-1.31659189159709));
#22345=CARTESIAN_POINT('Ctrl Pts',(92.7743366053888,-1.11394873342593,-1.38786342467876));
#22346=CARTESIAN_POINT('Ctrl Pts',(92.7829703475025,-1.004454293915,-1.46517557485391));
#22347=CARTESIAN_POINT('Ctrl Pts',(92.7845671229953,-0.984089734457473,
-1.47893042232661));
#22348=CARTESIAN_POINT('Ctrl Pts',(92.7872053233213,-0.950314011132547,
-1.50073705851073));
#22349=CARTESIAN_POINT('Ctrl Pts',(92.7882373283492,-0.93706985563731,-1.50904224530852));
#22350=CARTESIAN_POINT('Ctrl Pts',(92.7901125573652,-0.912959694795034,
-1.52372153222333));
#22351=CARTESIAN_POINT('Ctrl Pts',(92.7909534595059,-0.902132115214952,
-1.53015696734714));
#22352=CARTESIAN_POINT('Ctrl Pts',(92.7927740639245,-0.878661982245547,
-1.5437708792748));
#22353=CARTESIAN_POINT('Ctrl Pts',(92.7937551012006,-0.865997981439144,
-1.5509103394321));
#22354=CARTESIAN_POINT('Ctrl Pts',(92.7965060246811,-0.830449568001355,
-1.57037997492746));
#22355=CARTESIAN_POINT('Ctrl Pts',(92.7982879630477,-0.807380809313508,
-1.58236400828553));
#22356=CARTESIAN_POINT('Ctrl Pts',(92.806037902137,-0.706922612689067,-1.63178254653194));
#22357=CARTESIAN_POINT('Ctrl Pts',(92.8121753595661,-0.627144916999823,
-1.66407312106551));
#22358=CARTESIAN_POINT('Ctrl Pts',(92.8282280318317,-0.416755723598562,
-1.73194610749768));
#22359=CARTESIAN_POINT('Ctrl Pts',(92.8382670207413,-0.283842019951991,
-1.75862416509129));
#22360=CARTESIAN_POINT('Ctrl Pts',(92.8489426755887,-0.131967366970449,
-1.77142520258336));
#22361=CARTESIAN_POINT('Ctrl Pts',(92.8501424455267,-0.114728114753844,
-1.77262521407942));
#22362=CARTESIAN_POINT('Ctrl Pts',(92.8519258152171,-0.0888058587637963,
-1.7740498678591));
#22363=CARTESIAN_POINT('Ctrl Pts',(92.8525188829277,-0.0801347964154283,
-1.77446268954428));
#22364=CARTESIAN_POINT('Ctrl Pts',(92.8535427350123,-0.0650713359090129,
-1.77506920303215));
#22365=CARTESIAN_POINT('Ctrl Pts',(92.8539750720542,-0.0586805910574123,
-1.77529196069697));
#22366=CARTESIAN_POINT('Ctrl Pts',(92.8549972763407,-0.043499770451354,
-1.77573904058176));
#22367=CARTESIAN_POINT('Ctrl Pts',(92.8555854417489,-0.0347090632694041,
-1.77593261679578));
#22368=CARTESIAN_POINT('Ctrl Pts',(92.8573576629775,-0.00806599157180379,
-1.77632140402357));
#22369=CARTESIAN_POINT('Ctrl Pts',(92.8585311648445,0.00978882064814059,
-1.77631276228262));
#22370=CARTESIAN_POINT('Ctrl Pts',(92.8644538701237,0.10078924922353,-1.77489647848007));
#22371=CARTESIAN_POINT('Ctrl Pts',(92.8690157025129,0.173805461101921,-1.76923995003621));
#22372=CARTESIAN_POINT('Ctrl Pts',(92.8819226752765,0.380990431400312,-1.7402342419735));
#22373=CARTESIAN_POINT('Ctrl Pts',(92.8901417484114,0.513086004069158,-1.70596288561294));
#22374=CARTESIAN_POINT('Ctrl Pts',(92.9009428844723,0.670493073098504,-1.64516668689581));
#22375=CARTESIAN_POINT('Ctrl Pts',(92.9030606670229,0.700678502751117,-1.63253906780276));
#22376=CARTESIAN_POINT('Ctrl Pts',(92.9062453815342,0.744937988223441,-1.61257014221255));
#22377=CARTESIAN_POINT('Ctrl Pts',(92.9072908592143,0.759291152228356,-1.60586175896308));
#22378=CARTESIAN_POINT('Ctrl Pts',(92.9091804995949,0.784904880870786,-1.59347024957454));
#22379=CARTESIAN_POINT('Ctrl Pts',(92.9100221759129,0.796198405856377,-1.58785742203266));
#22380=CARTESIAN_POINT('Ctrl Pts',(92.9118332624201,0.82024717163652,-1.57558423321915));
#22381=CARTESIAN_POINT('Ctrl Pts',(92.9128038837592,0.832983093777067,-1.56888821869952));
#22382=CARTESIAN_POINT('Ctrl Pts',(92.9154944337239,0.867858883395908,-1.55000761916097));
#22383=CARTESIAN_POINT('Ctrl Pts',(92.9172255664099,0.889821496161764,-1.53750455324515));
#22384=CARTESIAN_POINT('Ctrl Pts',(92.9265825735306,1.00594600170679,-1.4680746381808));
#22385=CARTESIAN_POINT('Ctrl Pts',(92.9345044964078,1.09491681564403,-1.40296834600878));
#22386=CARTESIAN_POINT('Ctrl Pts',(92.9507684492121,1.261700320557,-1.25534304369367));
#22387=CARTESIAN_POINT('Ctrl Pts',(92.9590771381228,1.33881923461502,-1.17274920566313));
#22388=CARTESIAN_POINT('Ctrl Pts',(92.9681488101624,1.41784771484333,-1.07007225831311));
#22389=CARTESIAN_POINT('Ctrl Pts',(92.9693160168416,1.42791405245832,-1.05660223861011));
#22390=CARTESIAN_POINT('Ctrl Pts',(92.9710685270796,1.44289362569969,-1.03595253286846));
#22391=CARTESIAN_POINT('Ctrl Pts',(92.9716626114668,1.44794760102437,-1.0288767750056));
#22392=CARTESIAN_POINT('Ctrl Pts',(92.9726874417418,1.45662760961242,-1.01653379318001));
#22393=CARTESIAN_POINT('Ctrl Pts',(92.9731197524237,1.46027735690318,-1.01128383251189));
#22394=CARTESIAN_POINT('Ctrl Pts',(92.9741409257841,1.46887000479777,-0.998780261454234));
#22395=CARTESIAN_POINT('Ctrl Pts',(92.9747280986733,1.47378758752764,-0.991509584760297));
#22396=CARTESIAN_POINT('Ctrl Pts',(92.9764941560305,1.48849959716133,-0.969406481638364));
#22397=CARTESIAN_POINT('Ctrl Pts',(92.9776625937753,1.49812581509776,-0.954462717259428));
#22398=CARTESIAN_POINT('Ctrl Pts',(92.9835331813231,1.54582731357498,-0.877910566718759));
#22399=CARTESIAN_POINT('Ctrl Pts',(92.9880516045662,1.58033745437071,-0.814152859592063));
#22400=CARTESIAN_POINT('Ctrl Pts',(93.0007769139332,1.66722499257112,-0.627150462620073));
#22401=CARTESIAN_POINT('Ctrl Pts',(93.0088578646156,1.70970251470316,-0.499872162206162));
#22402=CARTESIAN_POINT('Ctrl Pts',(93.0196222502321,1.74471640461645,-0.335019313572613));
#22403=CARTESIAN_POINT('Ctrl Pts',(93.0218695209038,1.75094016173377,-0.300801539050298));
#22404=CARTESIAN_POINT('Ctrl Pts',(93.0252105521052,1.75858696203341,-0.250397201374686));
#22405=CARTESIAN_POINT('Ctrl Pts',(93.0262795593992,1.76079890823176,-0.234337443227318));
#22406=CARTESIAN_POINT('Ctrl Pts',(93.0281949261588,1.76434459485241,-0.205699181151343));
#22407=CARTESIAN_POINT('Ctrl Pts',(93.0290385118307,1.76576439394069,-0.193132320955662));
#22408=CARTESIAN_POINT('Ctrl Pts',(93.0308357108636,1.76848920871186,-0.166464696108202));
#22409=CARTESIAN_POINT('Ctrl Pts',(93.0317903400181,1.76976002827542,-0.152361407354624));
#22410=CARTESIAN_POINT('Ctrl Pts',(93.0343890140194,1.77274330016713,-0.114146850572733));
#22411=CARTESIAN_POINT('Ctrl Pts',(93.036043024397,1.77413237049621,-0.0900141281322493));
#22412=CARTESIAN_POINT('Ctrl Pts',(93.0381340219422,1.77525508472944,-0.0597559735022117));
#22413=CARTESIAN_POINT('Ctrl Pts',(93.0385568852539,1.77545011806415,-0.0536494645266197));
#22414=CARTESIAN_POINT('Ctrl Pts',(93.0389806716583,1.77561363839032,-0.047542293405874));
#22415=CARTESIAN_POINT('Origin',(88.3562164250559,0.,0.));
#22416=CARTESIAN_POINT('',(93.9380452419004,1.77561363831514,-0.0475422962136777));
#22417=CARTESIAN_POINT('',(93.7915308001226,1.77561363900531,-0.0475422704373303));
#22418=CARTESIAN_POINT('',(88.3562164250559,1.77561363837197,-0.0475422940912398));
#22419=CARTESIAN_POINT('Ctrl Pts',(93.9380452419004,1.77561363825831,-0.0475422983361156));
#22420=CARTESIAN_POINT('Ctrl Pts',(93.932064216968,1.77342400896609,-0.129320751841116));
#22421=CARTESIAN_POINT('Ctrl Pts',(93.9261040070707,1.76558700019008,-0.210863377491231));
#22422=CARTESIAN_POINT('Ctrl Pts',(93.9190812768447,1.74915389466268,-0.309610326783592));
#22423=CARTESIAN_POINT('Ctrl Pts',(93.9178110419327,1.74587644207947,-0.327587264195588));
#22424=CARTESIAN_POINT('Ctrl Pts',(93.9159413667903,1.74058590020062,-0.354266068078609));
#22425=CARTESIAN_POINT('Ctrl Pts',(93.91533121331,1.73878377173417,-0.363007888016686));
#22426=CARTESIAN_POINT('Ctrl Pts',(93.9142373160668,1.7354143951053,-0.378751113415867));
#22427=CARTESIAN_POINT('Ctrl Pts',(93.9137523340385,1.73387055425268,-0.385756962503964));
#22428=CARTESIAN_POINT('Ctrl Pts',(93.9126570636886,1.73027011386946,-0.401637109181372));
#22429=CARTESIAN_POINT('Ctrl Pts',(93.9120482378743,1.72818765190767,-0.410505156209504));
#22430=CARTESIAN_POINT('Ctrl Pts',(93.9101643333073,1.72149364249509,-0.438057115724141));
#22431=CARTESIAN_POINT('Ctrl Pts',(93.9089017361248,1.71664645406548,-0.456683066593837));
#22432=CARTESIAN_POINT('Ctrl Pts',(93.90591523603,1.70433858489328,-0.501008964669987));
#22433=CARTESIAN_POINT('Ctrl Pts',(93.9042039922161,1.69659787990215,-0.526626793382687));
#22434=CARTESIAN_POINT('Ctrl Pts',(93.8974529160954,1.66343481159347,-0.62804411997303));
#22435=CARTESIAN_POINT('Ctrl Pts',(93.8925618212592,1.63348585505973,-0.702268062299535));
#22436=CARTESIAN_POINT('Ctrl Pts',(93.8809715838332,1.55118372057922,-0.872207090092294));
#22437=CARTESIAN_POINT('Ctrl Pts',(93.874272408138,1.49482937438349,-0.965607449451407));
#22438=CARTESIAN_POINT('Ctrl Pts',(93.8656731771968,1.41565681372803,-1.07312085861627));
#22439=CARTESIAN_POINT('Ctrl Pts',(93.8640703636354,1.40061768571666,-1.09267680249015));
#22440=CARTESIAN_POINT('Ctrl Pts',(93.861418855841,1.37532214927653,-1.12418898498729));
#22441=CARTESIAN_POINT('Ctrl Pts',(93.8603796150051,1.36530503797323,-1.13633358434851));
#22442=CARTESIAN_POINT('Ctrl Pts',(93.8584887546109,1.34690442392916,-1.15804764228581));
#22443=CARTESIAN_POINT('Ctrl Pts',(93.8576394664736,1.3385769371677,-1.16766332382448));
#22444=CARTESIAN_POINT('Ctrl Pts',(93.8557976223561,1.32038746768316,-1.18821625067455));
#22445=CARTESIAN_POINT('Ctrl Pts',(93.8548036708995,1.31049136404233,-1.19912188086078));
#22446=CARTESIAN_POINT('Ctrl Pts',(93.8520066669708,1.2824285230712,-1.22928515362792));
#22447=CARTESIAN_POINT('Ctrl Pts',(93.8501910566705,1.26396582768971,-1.24826085435847));
#22448=CARTESIAN_POINT('Ctrl Pts',(93.8422084260967,1.18177136168752,-1.32904546997689));
#22449=CARTESIAN_POINT('Ctrl Pts',(93.8358602738192,1.1138888730116,-1.38643171477092));
#22450=CARTESIAN_POINT('Ctrl Pts',(93.8224679770277,0.964697794219947,-1.49450194901544));
#22451=CARTESIAN_POINT('Ctrl Pts',(93.8154283348047,0.882995729582544,-1.54418152978826));
#22452=CARTESIAN_POINT('Ctrl Pts',(93.8053773149932,0.758325683220617,-1.60684409208148));
#22453=CARTESIAN_POINT('Ctrl Pts',(93.8022430019592,0.718227858245852,-1.6251631357424));
#22454=CARTESIAN_POINT('Ctrl Pts',(93.7983047182628,0.665801556143529,-1.64679450459689));
#22455=CARTESIAN_POINT('Ctrl Pts',(93.7974331205392,0.654064777535289,-1.65149118750045));
#22456=CARTESIAN_POINT('Ctrl Pts',(93.7960379210879,0.635044049802805,-1.6588680857658));
#22457=CARTESIAN_POINT('Ctrl Pts',(93.795509938176,0.627791172951811,-1.66162646830613));
#22458=CARTESIAN_POINT('Ctrl Pts',(93.7944779178436,0.613501445865366,-1.66695415364624));
#22459=CARTESIAN_POINT('Ctrl Pts',(93.7939737213439,0.606466034953206,-1.66952661740373));
#22460=CARTESIAN_POINT('Ctrl Pts',(93.7927099653469,0.588701764907681,-1.67589492649203));
#22461=CARTESIAN_POINT('Ctrl Pts',(93.7919537529158,0.577952071837437,-1.67963239794334));
#22462=CARTESIAN_POINT('Ctrl Pts',(93.7889032835193,0.534139226941025,-1.69439488180496));
#22463=CARTESIAN_POINT('Ctrl Pts',(93.7866540261119,0.500788615839324,-1.70454975542391));
#22464=CARTESIAN_POINT('Ctrl Pts',(93.7803590766397,0.405257858930089,-1.7305913803883));
#22465=CARTESIAN_POINT('Ctrl Pts',(93.7763965102849,0.342484219541614,-1.7441003834496));
#22466=CARTESIAN_POINT('Ctrl Pts',(93.764318786301,0.148456156966097,-1.77497277442892));
#22467=CARTESIAN_POINT('Ctrl Pts',(93.7562682297953,0.0158998081696953,
-1.78109817790297));
#22468=CARTESIAN_POINT('Ctrl Pts',(93.7460632877515,-0.141988959481852,
-1.77075581746317));
#22469=CARTESIAN_POINT('Ctrl Pts',(93.7443744812903,-0.167833692495375,
-1.76849336144285));
#22470=CARTESIAN_POINT('Ctrl Pts',(93.7416967620832,-0.208297311049322,
-1.764056220399));
#22471=CARTESIAN_POINT('Ctrl Pts',(93.74071982405,-0.222955011140102,-1.76226364639208));
#22472=CARTESIAN_POINT('Ctrl Pts',(93.7388907482296,-0.250191254348781,
-1.75858753744992));
#22473=CARTESIAN_POINT('Ctrl Pts',(93.738040157464,-0.262775290960008,-1.75675124094689));
#22474=CARTESIAN_POINT('Ctrl Pts',(93.7361304787226,-0.290838456750996,
-1.75234791812534));
#22475=CARTESIAN_POINT('Ctrl Pts',(93.7350692228578,-0.306305309374883,
-1.74971062291305));
#22476=CARTESIAN_POINT('Ctrl Pts',(93.7318657030709,-0.352596240795009,
-1.74118485278453));
#22477=CARTESIAN_POINT('Ctrl Pts',(93.7297043162238,-0.383299832116641,
-1.73468435794648));
#22478=CARTESIAN_POINT('Ctrl Pts',(93.7206554325429,-0.509611182069572,
-1.70442493991075));
#22479=CARTESIAN_POINT('Ctrl Pts',(93.7135523773192,-0.603320151802286,
-1.67354940206419));
#22480=CARTESIAN_POINT('Ctrl Pts',(93.6980298144184,-0.799045927245915,
-1.59047738940703));
#22481=CARTESIAN_POINT('Ctrl Pts',(93.6896133338755,-0.899580743631573,
-1.53585513859791));
#22482=CARTESIAN_POINT('Ctrl Pts',(93.6804485128342,-1.00806719754256,-1.46258171375491));
#22483=CARTESIAN_POINT('Ctrl Pts',(93.6792856212177,-1.0218179624261,-1.45300820598767));
#22484=CARTESIAN_POINT('Ctrl Pts',(93.6775347847855,-1.04252738539006,-1.4381505396072));
#22485=CARTESIAN_POINT('Ctrl Pts',(93.6769381694574,-1.04958550466908,-1.43300753674767));
#22486=CARTESIAN_POINT('Ctrl Pts',(93.6759062149524,-1.06180067900675,-1.42396809982054));
#22487=CARTESIAN_POINT('Ctrl Pts',(93.6754693236448,-1.06697466237805,-1.42009538560277));
#22488=CARTESIAN_POINT('Ctrl Pts',(93.674433167974,-1.07925086259638,-1.41080170758836));
#22489=CARTESIAN_POINT('Ctrl Pts',(93.6738356808908,-1.08633346065656,-1.40535529436161));
#22490=CARTESIAN_POINT('Ctrl Pts',(93.6720237361292,-1.10781112677829,-1.38857989178399));
#22491=CARTESIAN_POINT('Ctrl Pts',(93.6708204332204,-1.122072809844,-1.37708107320852));
#22492=CARTESIAN_POINT('Ctrl Pts',(93.6646287406169,-1.19526853983663,-1.31617297336947));
#22493=CARTESIAN_POINT('Ctrl Pts',(93.6598464708331,-1.25113231978726,-1.2631899063244));
#22494=CARTESIAN_POINT('Ctrl Pts',(93.6461755011858,-1.40187971177965,-1.10036971653318));
#22495=CARTESIAN_POINT('Ctrl Pts',(93.6374037849479,-1.48696623616425,-0.982348083167489));
#22496=CARTESIAN_POINT('Ctrl Pts',(93.6264415414659,-1.56863900284259,-0.833692832635021));
#22497=CARTESIAN_POINT('Ctrl Pts',(93.624833548212,-1.5800604031398,-0.811838090916207));
#22498=CARTESIAN_POINT('Ctrl Pts',(93.622264443553,-1.59740379672548,-0.77689841321814));
#22499=CARTESIAN_POINT('Ctrl Pts',(93.6213139409969,-1.60362863692112,-0.763966758907573));
#22500=CARTESIAN_POINT('Ctrl Pts',(93.6195075397764,-1.61509352061627,-0.739391625501737));
#22501=CARTESIAN_POINT('Ctrl Pts',(93.6186528350781,-1.62036607857833,-0.727764256389499));
#22502=CARTESIAN_POINT('Ctrl Pts',(93.6166969355332,-1.632084061398,-0.701164302350791));
#22503=CARTESIAN_POINT('Ctrl Pts',(93.6155930937495,-1.63844955509484,-0.686157989688276));
#22504=CARTESIAN_POINT('Ctrl Pts',(93.6121149429335,-1.657729938153,-0.638906851947309));
#22505=CARTESIAN_POINT('Ctrl Pts',(93.60971631391,-1.66990544092752,-0.606371205076973));
#22506=CARTESIAN_POINT('Ctrl Pts',(93.5958472210486,-1.73395018128646,-0.418635307898377));
#22507=CARTESIAN_POINT('Ctrl Pts',(93.5837104342289,-1.76512212983418,-0.25722489164812));
#22508=CARTESIAN_POINT('Ctrl Pts',(93.5682221334524,-1.77644160955396,-0.0433518631493959));
#22509=CARTESIAN_POINT('Ctrl Pts',(93.564608095318,-1.77695590541709,0.00727127327235955));
#22510=CARTESIAN_POINT('Ctrl Pts',(93.560174877126,-1.77487894761392,0.0710073011846654));
#22511=CARTESIAN_POINT('Ctrl Pts',(93.5592664760859,-1.77430401511516,0.0841582040911155));
#22512=CARTESIAN_POINT('Ctrl Pts',(93.5578269487021,-1.7731516629115,0.105162834718707));
#22513=CARTESIAN_POINT('Ctrl Pts',(93.5572909506516,-1.77266813518198,0.113020927663279));
#22514=CARTESIAN_POINT('Ctrl Pts',(93.5562557660819,-1.77162767430701,0.128274893734556));
#22515=CARTESIAN_POINT('Ctrl Pts',(93.5557562975695,-1.7710766448611,0.135670870770977));
#22516=CARTESIAN_POINT('Ctrl Pts',(93.5545220997813,-1.7695931518056,0.154029834762301));
#22517=CARTESIAN_POINT('Ctrl Pts',(93.5537903901603,-1.76860510070327,0.164988260380485));
#22518=CARTESIAN_POINT('Ctrl Pts',(93.5509731565614,-1.76438019789977,0.207432851803631));
#22519=CARTESIAN_POINT('Ctrl Pts',(93.548924408518,-1.76040362424818,0.23884145600169));
#22520=CARTESIAN_POINT('Ctrl Pts',(93.543404046258,-1.74724592875639,0.324354284080489));
#22521=CARTESIAN_POINT('Ctrl Pts',(93.5399930567425,-1.73639401043948,0.37816755531454));
#22522=CARTESIAN_POINT('Ctrl Pts',(93.5280587394473,-1.68939917133564,0.565873043702462));
#22523=CARTESIAN_POINT('Ctrl Pts',(93.5196813388008,-1.6401076225318,0.695935467971167));
#22524=CARTESIAN_POINT('Ctrl Pts',(93.5088562955244,-1.56233175632845,0.845628750530105));
#22525=CARTESIAN_POINT('Ctrl Pts',(93.5069060880123,-1.54779135251087,0.871957716502482));
#22526=CARTESIAN_POINT('Ctrl Pts',(93.5039064464908,-1.52468859299561,0.91139074682668));
#22527=CARTESIAN_POINT('Ctrl Pts',(93.5028743129305,-1.51660943717015,0.924772506087227));
#22528=CARTESIAN_POINT('Ctrl Pts',(93.5009909083532,-1.50164055397037,0.948842114339685));
#22529=CARTESIAN_POINT('Ctrl Pts',(93.5001418808112,-1.49481060048346,0.959566029770632));
#22530=CARTESIAN_POINT('Ctrl Pts',(93.4982942950274,-1.47977513833724,0.982623543970468));
#22531=CARTESIAN_POINT('Ctrl Pts',(93.4972942696386,-1.4715293371001,0.99492958346697));
#22532=CARTESIAN_POINT('Ctrl Pts',(93.4944616961243,-1.44787832792654,1.02928909489754));
#22533=CARTESIAN_POINT('Ctrl Pts',(93.4926160676028,-1.43212523293026,1.05109698531739));
#22534=CARTESIAN_POINT('Ctrl Pts',(93.4843708327006,-1.36028536199637,1.14593458366941));
#22535=CARTESIAN_POINT('Ctrl Pts',(93.4777755866483,-1.29907227904524,1.21488643308539));
#22536=CARTESIAN_POINT('Ctrl Pts',(93.4636616329492,-1.15946108251805,1.34947827119889));
#22537=CARTESIAN_POINT('Ctrl Pts',(93.456143853353,-1.08017482561964,1.41374140241039));
#22538=CARTESIAN_POINT('Ctrl Pts',(93.4463221822853,-0.966532815612609,
1.4906807011022));
#22539=CARTESIAN_POINT('Ctrl Pts',(93.4438221933532,-0.936661568546289,
1.50962913814869));
#22540=CARTESIAN_POINT('Ctrl Pts',(93.4405544940258,-0.896110940857078,
1.53368445529899));
#22541=CARTESIAN_POINT('Ctrl Pts',(93.4397435695085,-0.885919748459911,
1.53959379218729));
#22542=CARTESIAN_POINT('Ctrl Pts',(93.4384726747304,-0.869733103171513,
1.54876562395411));
#22543=CARTESIAN_POINT('Ctrl Pts',(93.4380086083511,-0.863776562230541,
1.55209557799372));
#22544=CARTESIAN_POINT('Ctrl Pts',(93.4370408123907,-0.851254522718967,
1.55900150379228));
#22545=CARTESIAN_POINT('Ctrl Pts',(93.436537565545,-0.844685385861342,1.56257049546946));
#22546=CARTESIAN_POINT('Ctrl Pts',(93.4352796184397,-0.828125200432104,
1.57143264153487));
#22547=CARTESIAN_POINT('Ctrl Pts',(93.4345282005413,-0.818105559289383,
1.57667219324101));
#22548=CARTESIAN_POINT('Ctrl Pts',(93.4315250359133,-0.777579800567155,
1.59737389586408));
#22549=CARTESIAN_POINT('Ctrl Pts',(93.4293165488909,-0.746677998174211,
1.61205025819796));
#22550=CARTESIAN_POINT('Ctrl Pts',(93.4231848078267,-0.658459581322483,
1.65086667977955));
#22551=CARTESIAN_POINT('Ctrl Pts',(93.4193396320445,-0.600270196795669,
1.67290363377777));
#22552=CARTESIAN_POINT('Ctrl Pts',(93.4071631902648,-0.411708830257406,
1.73320438443527));
#22553=CARTESIAN_POINT('Ctrl Pts',(93.3989135625157,-0.278074791546838,
1.75959425939188));
#22554=CARTESIAN_POINT('Ctrl Pts',(93.3885033343085,-0.117266968741904,
1.77255911488489));
#22555=CARTESIAN_POINT('Ctrl Pts',(93.3868387516293,-0.091749743853286,
1.77406291742127));
#22556=CARTESIAN_POINT('Ctrl Pts',(93.3841909620317,-0.0515359169358551,
1.77556293580235));
#22557=CARTESIAN_POINT('Ctrl Pts',(93.3832192815249,-0.0368560317405538,
1.77592829271832));
#22558=CARTESIAN_POINT('Ctrl Pts',(93.3813949405143,-0.00945079146547175,
1.77627043037224));
#22559=CARTESIAN_POINT('Ctrl Pts',(93.3805437583539,0.00327312796116224,
1.7762925523013));
#22560=CARTESIAN_POINT('Ctrl Pts',(93.3786260024962,0.0317936252256098,
1.77603570235679));
#22561=CARTESIAN_POINT('Ctrl Pts',(93.3775571756645,0.0475882793237433,
1.77568267946322));
#22562=CARTESIAN_POINT('Ctrl Pts',(93.3743059484304,0.0953160979571939,
1.77397869043863));
#22563=CARTESIAN_POINT('Ctrl Pts',(93.3721035673673,0.127217980976721,1.77197655411225));
#22564=CARTESIAN_POINT('Ctrl Pts',(93.3583083801192,0.324308754421789,1.75425772207082));
#22565=CARTESIAN_POINT('Ctrl Pts',(93.3460112670075,0.486656738414632,1.71631634661313));
#22566=CARTESIAN_POINT('Ctrl Pts',(93.3302160596375,0.690152138386397,1.63752688002723));
#22567=CARTESIAN_POINT('Ctrl Pts',(93.3264731440086,0.738113413084914,1.61647577076743));
#22568=CARTESIAN_POINT('Ctrl Pts',(93.3219094459022,0.79698626544526,1.58746753174659));
#22569=CARTESIAN_POINT('Ctrl Pts',(93.3209931537949,0.808827980177294,1.58146691291037));
#22570=CARTESIAN_POINT('Ctrl Pts',(93.3195441289377,0.827605422254967,1.57168562023021));
#22571=CARTESIAN_POINT('Ctrl Pts',(93.319006416856,0.834584864468106,1.56799060390182));
#22572=CARTESIAN_POINT('Ctrl Pts',(93.3179704197863,0.848058580154164,1.56074197225628));
#22573=CARTESIAN_POINT('Ctrl Pts',(93.3174718273927,0.854555611178217,1.55719413337679));
#22574=CARTESIAN_POINT('Ctrl Pts',(93.3162433146843,0.870589558154492,1.54830789216091));
#22575=CARTESIAN_POINT('Ctrl Pts',(93.3155163515095,0.880099950627387,1.54292177368071));
#22576=CARTESIAN_POINT('Ctrl Pts',(93.312741991114,0.916450523592709,1.5218895004793));
#22577=CARTESIAN_POINT('Ctrl Pts',(93.3107299544161,0.942929867873822,1.50562703030943));
#22578=CARTESIAN_POINT('Ctrl Pts',(93.3053443244942,1.01362306236464,1.45961326572982));
#22579=CARTESIAN_POINT('Ctrl Pts',(93.302027819328,1.05694824863634,1.42855303378692));
#22580=CARTESIAN_POINT('Ctrl Pts',(93.2905649303247,1.2028616076847,1.31366853968444));
#22581=CARTESIAN_POINT('Ctrl Pts',(93.2825652740839,1.2974146084182,1.22037476729893));
#22582=CARTESIAN_POINT('Ctrl Pts',(93.2720476895369,1.40113835850593,1.09221276734445));
#22583=CARTESIAN_POINT('Ctrl Pts',(93.2699547525255,1.42085984449617,1.06643074083501));
#22584=CARTESIAN_POINT('Ctrl Pts',(93.2667838138539,1.44928484549225,1.02708148635314));
#22585=CARTESIAN_POINT('Ctrl Pts',(93.2657263319464,1.45852866177532,1.01391176035958));
#22586=CARTESIAN_POINT('Ctrl Pts',(93.2638747197923,1.47429708362159,0.990784456891326));
#22587=CARTESIAN_POINT('Ctrl Pts',(93.2630837143151,1.48090295627574,0.980883353485329));
#22588=CARTESIAN_POINT('Ctrl Pts',(93.2614149077411,1.49456336596262,0.959956110432165));
#22589=CARTESIAN_POINT('Ctrl Pts',(93.2605363710762,1.50159649830148,0.948916924290748));
#22590=CARTESIAN_POINT('Ctrl Pts',(93.2584080895476,1.51825042759562,0.92212812921801));
#22591=CARTESIAN_POINT('Ctrl Pts',(93.25715395688,1.52774884051114,0.906304630340698));
#22592=CARTESIAN_POINT('Ctrl Pts',(93.2525459688191,1.56149398299845,0.848049983425419));
#22593=CARTESIAN_POINT('Ctrl Pts',(93.2491394620652,1.58423151366537,0.804774472179879));
#22594=CARTESIAN_POINT('Ctrl Pts',(93.2399716105195,1.63966345229121,0.687795151691299));
#22595=CARTESIAN_POINT('Ctrl Pts',(93.2341238888131,1.66917312532955,0.612712951792597));
#22596=CARTESIAN_POINT('Ctrl Pts',(93.2204713262312,1.7255377664724,0.43459480648691));
#22597=CARTESIAN_POINT('Ctrl Pts',(93.2126582125065,1.74844221397177,0.330615576841279));
#22598=CARTESIAN_POINT('Ctrl Pts',(93.2039837022445,1.76413778331815,0.207819983310635));
#22599=CARTESIAN_POINT('Ctrl Pts',(93.2027663351122,1.7661026566286,0.190401491911574));
#22600=CARTESIAN_POINT('Ctrl Pts',(93.2009587090377,1.76866447420252,0.164216762282819));
#22601=CARTESIAN_POINT('Ctrl Pts',(93.2003587061771,1.76945469378544,0.155471097681425));
#22602=CARTESIAN_POINT('Ctrl Pts',(93.1993235127337,1.77071367410087,0.140281441403671));
#22603=CARTESIAN_POINT('Ctrl Pts',(93.1988867291409,1.77121216870269,0.1338404093729));
#22604=CARTESIAN_POINT('Ctrl Pts',(93.1978540964208,1.77231258804181,0.118537110675026));
#22605=CARTESIAN_POINT('Ctrl Pts',(93.1972599832262,1.7728831956536,0.109672874277451));
#22606=CARTESIAN_POINT('Ctrl Pts',(93.1954691157638,1.77441151937427,0.082786078274788));
#22607=CARTESIAN_POINT('Ctrl Pts',(93.1942831416912,1.7751611148671,0.0647522416044393));
#22608=CARTESIAN_POINT('Ctrl Pts',(93.1910644008543,1.77646221521149,0.015291391870698));
#22609=CARTESIAN_POINT('Ctrl Pts',(93.1890567017321,1.77645452257652,-0.0161368862966694));
#22610=CARTESIAN_POINT('Ctrl Pts',(93.1870734170205,1.77561363809212,-0.0475423045429159));
#22611=CARTESIAN_POINT('Ctrl Pts',(93.0389806716583,1.77561363839032,-0.047542293405874));
#22612=CARTESIAN_POINT('Ctrl Pts',(93.0406142785543,1.77624397463933,-0.0240004412921055));
#22613=CARTESIAN_POINT('Ctrl Pts',(93.0422616476878,1.77640604792239,-0.000448753302874027));
#22614=CARTESIAN_POINT('Ctrl Pts',(93.0486331855031,1.77523068615551,0.0899260868132504));
#22615=CARTESIAN_POINT('Ctrl Pts',(93.0534448008932,1.77059074467301,0.156644745852565));
#22616=CARTESIAN_POINT('Ctrl Pts',(93.0656822186869,1.74948528761673,0.323472131199964));
#22617=CARTESIAN_POINT('Ctrl Pts',(93.0731601714229,1.72818673807063,0.422734339993162));
#22618=CARTESIAN_POINT('Ctrl Pts',(93.0830061780318,1.68796328643129,0.554212140705317));
#22619=CARTESIAN_POINT('Ctrl Pts',(93.0855633978304,1.67633262754556,0.588456023419935));
#22620=CARTESIAN_POINT('Ctrl Pts',(93.0888879996843,1.65952821414169,0.63337943210798));
#22621=CARTESIAN_POINT('Ctrl Pts',(93.08970069677,1.65528231549723,0.644394191123166));
#22622=CARTESIAN_POINT('Ctrl Pts',(93.0909706465522,1.64842388787623,0.661671191850491));
#22623=CARTESIAN_POINT('Ctrl Pts',(93.091432041536,1.6458848409825,0.667961955793922));
#22624=CARTESIAN_POINT('Ctrl Pts',(93.0923901448549,1.64051209253187,0.6810568688574));
#22625=CARTESIAN_POINT('Ctrl Pts',(93.092886415574,1.63767198186023,0.687858173508663));
#22626=CARTESIAN_POINT('Ctrl Pts',(93.0941195709511,1.63047380726,0.704798562713444));
#22627=CARTESIAN_POINT('Ctrl Pts',(93.0948533729094,1.62606333629056,0.714915304100834));
#22628=CARTESIAN_POINT('Ctrl Pts',(93.097725857473,1.60830876588358,0.754626271998064));
#22629=CARTESIAN_POINT('Ctrl Pts',(93.0998256718011,1.59424786945938,0.783895362317591));
#22630=CARTESIAN_POINT('Ctrl Pts',(93.1055471244885,1.55318058095326,0.86369869612356));
#22631=CARTESIAN_POINT('Ctrl Pts',(93.1091023449359,1.52451919295323,0.913338648689704));
#22632=CARTESIAN_POINT('Ctrl Pts',(93.1215850284528,1.41485156146095,1.0836847163296));
#22633=CARTESIAN_POINT('Ctrl Pts',(93.1303761840958,1.32151150240489,1.19573448139649));
#22634=CARTESIAN_POINT('Ctrl Pts',(93.1413352204001,1.19789011291407,1.31175887919233));
#22635=CARTESIAN_POINT('Ctrl Pts',(93.1429165699177,1.17987151840116,1.32798915189923));
#22636=CARTESIAN_POINT('Ctrl Pts',(93.1454555967787,1.15070050009218,1.35320257218564));
#22637=CARTESIAN_POINT('Ctrl Pts',(93.1464031659091,1.13976157589448,1.36242885032582));
#22638=CARTESIAN_POINT('Ctrl Pts',(93.1481126797813,1.11994161809837,1.37873995664914));
#22639=CARTESIAN_POINT('Ctrl Pts',(93.1488725757104,1.11110174388814,1.38587373176154));
#22640=CARTESIAN_POINT('Ctrl Pts',(93.1506667936614,1.09016453962537,1.40244096541801));
#22641=CARTESIAN_POINT('Ctrl Pts',(93.1517038725532,1.07801238571957,1.41180333452864));
#22642=CARTESIAN_POINT('Ctrl Pts',(93.1547897455314,1.04171626110587,1.4390250616293));
#22643=CARTESIAN_POINT('Ctrl Pts',(93.1568558100862,1.01723998919406,1.45643005664982));
#22644=CARTESIAN_POINT('Ctrl Pts',(93.1616930092813,0.959565114260596,1.49527924154872));
#22645=CARTESIAN_POINT('Ctrl Pts',(93.1644795358848,0.926069503570083,1.51625199095094));
#22646=CARTESIAN_POINT('Ctrl Pts',(93.1754864340768,0.79264514446526,1.59372261243583));
#22647=CARTESIAN_POINT('Ctrl Pts',(93.1839418669352,0.688038806069294,1.64159567293732));
#22648=CARTESIAN_POINT('Ctrl Pts',(93.197088608169,0.517299364806754,1.70053041041206));
#22649=CARTESIAN_POINT('Ctrl Pts',(93.2018332248535,0.453884512140813,1.71854386208169));
#22650=CARTESIAN_POINT('Ctrl Pts',(93.207380256267,0.37614108235373,1.73602203725509));
#22651=CARTESIAN_POINT('Ctrl Pts',(93.2083340204843,0.362637351062339,1.73889298372775));
#22652=CARTESIAN_POINT('Ctrl Pts',(93.2098247392325,0.341294153731156,1.74317117888793));
#22653=CARTESIAN_POINT('Ctrl Pts',(93.2103672280361,0.333476671794237,1.7446835741515));
#22654=CARTESIAN_POINT('Ctrl Pts',(93.2113982471524,0.318517420158293,1.74747341762132));
#22655=CARTESIAN_POINT('Ctrl Pts',(93.2118872261099,0.311377666597152,1.74875974415353));
#22656=CARTESIAN_POINT('Ctrl Pts',(93.2130717604991,0.293976992228449,1.75178477392434));
#22657=CARTESIAN_POINT('Ctrl Pts',(93.21376476097,0.283708094846553,1.75347714446922));
#22658=CARTESIAN_POINT('Ctrl Pts',(93.2162802638395,0.246135712383341,1.75933056339864));
#22659=CARTESIAN_POINT('Ctrl Pts',(93.2180751483871,0.218749562331486,1.7629451635433));
#22660=CARTESIAN_POINT('Ctrl Pts',(93.2227096208673,0.146899423847069,1.77072813619613));
#22661=CARTESIAN_POINT('Ctrl Pts',(93.2255095900357,0.102341807918322,1.77386139570429));
#22662=CARTESIAN_POINT('Ctrl Pts',(93.2370736032073,-0.0838922325888598,
1.77991537877549));
#22663=CARTESIAN_POINT('Ctrl Pts',(93.2455785451679,-0.22553060572245,1.76756116460121));
#22664=CARTESIAN_POINT('Ctrl Pts',(93.2570031888832,-0.401287777423312,
1.73074209958905));
#22665=CARTESIAN_POINT('Ctrl Pts',(93.2594440932583,-0.438117233915936,
1.72178775120697));
#22666=CARTESIAN_POINT('Ctrl Pts',(93.2629354818483,-0.489562397813883,
1.70752242608633));
#22667=CARTESIAN_POINT('Ctrl Pts',(93.2639548771397,-0.504439354457537,
1.70318674535118));
#22668=CARTESIAN_POINT('Ctrl Pts',(93.2658312884794,-0.531547261307627,
1.69490021202221));
#22669=CARTESIAN_POINT('Ctrl Pts',(93.2666862778402,-0.543795800889764,
1.69101015131005));
#22670=CARTESIAN_POINT('Ctrl Pts',(93.2684344849686,-0.568623976363802,
1.68282723111918));
#22671=CARTESIAN_POINT('Ctrl Pts',(93.2693279523319,-0.581199769257263,
1.67852540278963));
#22672=CARTESIAN_POINT('Ctrl Pts',(93.2715773640878,-0.612570379016939,
1.66739958569441));
#22673=CARTESIAN_POINT('Ctrl Pts',(93.2729391025499,-0.631300050194068,
1.66039875847731));
#22674=CARTESIAN_POINT('Ctrl Pts',(93.278682914961,-0.709185480412747,1.62977823698092));
#22675=CARTESIAN_POINT('Ctrl Pts',(93.2831588674551,-0.767160632073596,
1.60330409336184));
#22676=CARTESIAN_POINT('Ctrl Pts',(93.297749016221,-0.947781610391456,1.50878215246473));
#22677=CARTESIAN_POINT('Ctrl Pts',(93.3081697953428,-1.06383609902388,1.42932194886656));
#22678=CARTESIAN_POINT('Ctrl Pts',(93.3209500804986,-1.19797147017989,1.31201192604106));
#22679=CARTESIAN_POINT('Ctrl Pts',(93.3236443248948,-1.22579470575232,1.28605550140802));
#22680=CARTESIAN_POINT('Ctrl Pts',(93.3271157809467,-1.26128187343392,1.25075034695414));
#22681=CARTESIAN_POINT('Ctrl Pts',(93.3279432511827,-1.26971286354833,1.2421906692488));
#22682=CARTESIAN_POINT('Ctrl Pts',(93.3292819208889,-1.28331664506931,1.22809601373978));
#22683=CARTESIAN_POINT('Ctrl Pts',(93.329796968343,-1.28854186172002,1.22261249238358));
#22684=CARTESIAN_POINT('Ctrl Pts',(93.3308164614659,-1.29887028192478,1.21163372659912));
#22685=CARTESIAN_POINT('Ctrl Pts',(93.3313209432362,-1.30397406428339,1.20613927098943));
#22686=CARTESIAN_POINT('Ctrl Pts',(93.3326035601201,-1.31692671924963,1.1920168278806));
#22687=CARTESIAN_POINT('Ctrl Pts',(93.3333780641369,-1.324725843107,1.18334338234599));
#22688=CARTESIAN_POINT('Ctrl Pts',(93.3366631962968,-1.35767785559932,1.145963169055));
#22689=CARTESIAN_POINT('Ctrl Pts',(93.339119361292,-1.38198928905391,1.11652444281191));
#22690=CARTESIAN_POINT('Ctrl Pts',(93.3463101330933,-1.45139980505251,1.02673066215157));
#22691=CARTESIAN_POINT('Ctrl Pts',(93.3509305280875,-1.49363060060257,0.964264694474558));
#22692=CARTESIAN_POINT('Ctrl Pts',(93.3626478694777,-1.59028020971078,0.799642686601972));
#22693=CARTESIAN_POINT('Ctrl Pts',(93.3697367552534,-1.63891871868585,0.694522286231583));
#22694=CARTESIAN_POINT('Ctrl Pts',(93.3787567435776,-1.68506539264836,0.562331906409825));
#22695=CARTESIAN_POINT('Ctrl Pts',(93.3803466255576,-1.692650053789,0.539071658408503));
#22696=CARTESIAN_POINT('Ctrl Pts',(93.3829757995194,-1.70428075436109,0.500734023055078));
#22697=CARTESIAN_POINT('Ctrl Pts',(93.3840057839586,-1.7086128539619,0.48574637506263));
#22698=CARTESIAN_POINT('Ctrl Pts',(93.3858788744068,-1.71608414496795,0.458560648444357));
#22699=CARTESIAN_POINT('Ctrl Pts',(93.3867196832692,-1.71929211456859,0.44638242756821));
#22700=CARTESIAN_POINT('Ctrl Pts',(93.3885418269849,-1.72592949021877,0.420051769619085));
#22701=CARTESIAN_POINT('Ctrl Pts',(93.3895245162812,-1.72931487899894,0.405889297229369));
#22702=CARTESIAN_POINT('Ctrl Pts',(93.392285060387,-1.73828315310545,0.366220483378832));
#22703=CARTESIAN_POINT('Ctrl Pts',(93.3940751050549,-1.74347813766206,0.340631208172091));
#22704=CARTESIAN_POINT('Ctrl Pts',(93.4018936776905,-1.76350125577842,0.229490071266932));
#22705=CARTESIAN_POINT('Ctrl Pts',(93.4080952562282,-1.77260764200031,0.143040757421338));
#22706=CARTESIAN_POINT('Ctrl Pts',(93.424104297921,-1.77959104605296,-0.0772390947565849));
#22707=CARTESIAN_POINT('Ctrl Pts',(93.4340248105918,-1.76874811271193,-0.210814917675523));
#22708=CARTESIAN_POINT('Ctrl Pts',(93.4446186809813,-1.73964816193103,-0.35916181805912));
#22709=CARTESIAN_POINT('Ctrl Pts',(93.4458394396303,-1.73600918469313,-0.376357686041292));
#22710=CARTESIAN_POINT('Ctrl Pts',(93.4476474962382,-1.73017954805635,-0.402018848997123));
#22711=CARTESIAN_POINT('Ctrl Pts',(93.4482446376791,-1.72818078142562,-0.410526026340157));
#22712=CARTESIAN_POINT('Ctrl Pts',(93.4493207481165,-1.72444350544355,-0.425921496159045));
#22713=CARTESIAN_POINT('Ctrl Pts',(93.4498008501261,-1.72272639017773,-0.432814409202329));
#22714=CARTESIAN_POINT('Ctrl Pts',(93.4508912563302,-1.7187127185108,-0.448523855111298));
#22715=CARTESIAN_POINT('Ctrl Pts',(93.451500049308,-1.71638963534372,-0.457333233113122));
#22716=CARTESIAN_POINT('Ctrl Pts',(93.4534034045911,-1.70887087216756,-0.48498067230348));
#22717=CARTESIAN_POINT('Ctrl Pts',(93.4546850024889,-1.7034318598969,-0.503751809866261));
#22718=CARTESIAN_POINT('Ctrl Pts',(93.4577300252228,-1.68962964951911,-0.54860332533262));
#22719=CARTESIAN_POINT('Ctrl Pts',(93.4594800312124,-1.68097076911431,-0.574588021751886));
#22720=CARTESIAN_POINT('Ctrl Pts',(93.466515811897,-1.64335272897686,-0.679335583647343));
#22721=CARTESIAN_POINT('Ctrl Pts',(93.471639356881,-1.60942924039693,-0.756203922295841));
#22722=CARTESIAN_POINT('Ctrl Pts',(93.4831735720289,-1.52160944990598,-0.922263628436107));
#22723=CARTESIAN_POINT('Ctrl Pts',(93.489584903079,-1.46505874127027,-1.00968563248125));
#22724=CARTESIAN_POINT('Ctrl Pts',(93.497863123968,-1.38606887330017,-1.11107284058865));
#22725=CARTESIAN_POINT('Ctrl Pts',(93.4994623237408,-1.37054187152664,-1.13017019179927));
#22726=CARTESIAN_POINT('Ctrl Pts',(93.5021036978561,-1.3445048728511,-1.16086839592352));
#22727=CARTESIAN_POINT('Ctrl Pts',(93.5031364127707,-1.33422916091378,-1.17266419141022));
#22728=CARTESIAN_POINT('Ctrl Pts',(93.505012394501,-1.31540058506222,-1.19371019572356));
#22729=CARTESIAN_POINT('Ctrl Pts',(93.505853330792,-1.3069024821671,-1.20300815400473));
#22730=CARTESIAN_POINT('Ctrl Pts',(93.5076734013209,-1.288390654785,-1.22283469382464));
#22731=CARTESIAN_POINT('Ctrl Pts',(93.5086538637808,-1.2783452531001,-1.23333229899567));
#22732=CARTESIAN_POINT('Ctrl Pts',(93.5114014431643,-1.24999990051939,-1.2622352855805));
#22733=CARTESIAN_POINT('Ctrl Pts',(93.513180564556,-1.23142428719495,-1.28036392024195));
#22734=CARTESIAN_POINT('Ctrl Pts',(93.5209067693397,-1.14985390140676,-1.35655404644318));
#22735=CARTESIAN_POINT('Ctrl Pts',(93.5270220766126,-1.08310942369822,-1.41041594077166));
#22736=CARTESIAN_POINT('Ctrl Pts',(93.5430902851623,-0.901298634263778,
-1.53659654082754));
#22737=CARTESIAN_POINT('Ctrl Pts',(93.5531707714034,-0.781352520423305,
-1.60092441130058));
#22738=CARTESIAN_POINT('Ctrl Pts',(93.5638748452446,-0.63928758717903,-1.6573081732651));
#22739=CARTESIAN_POINT('Ctrl Pts',(93.5650671292812,-0.623233289410249,
-1.66341195196184));
#22740=CARTESIAN_POINT('Ctrl Pts',(93.566841682871,-0.59895402814274,-1.67224194591509));
#22741=CARTESIAN_POINT('Ctrl Pts',(93.5674332879617,-0.590794040287253,
-1.67514222184071));
#22742=CARTESIAN_POINT('Ctrl Pts',(93.5684557389121,-0.576571059152577,
-1.68008058781324));
#22743=CARTESIAN_POINT('Ctrl Pts',(93.5688881199724,-0.570517969440732,
-1.68214571825519));
#22744=CARTESIAN_POINT('Ctrl Pts',(93.5699118342719,-0.556095656455988,
-1.68697936678798));
#22745=CARTESIAN_POINT('Ctrl Pts',(93.5705014481086,-0.547716818794986,
-1.68971833681279));
#22746=CARTESIAN_POINT('Ctrl Pts',(93.5722826874621,-0.522197447845928,
-1.69785062848668));
#22747=CARTESIAN_POINT('Ctrl Pts',(93.5734636011663,-0.504994567596273,
-1.70304652867212));
#22748=CARTESIAN_POINT('Ctrl Pts',(93.5794633113212,-0.416325137294466,
-1.72836614199646));
#22749=CARTESIAN_POINT('Ctrl Pts',(93.5840892859787,-0.343719100184372,
-1.74425793981282));
#22750=CARTESIAN_POINT('Ctrl Pts',(93.5972697631542,-0.132483169000386,
-1.77678444263114));
#22751=CARTESIAN_POINT('Ctrl Pts',(93.6056984043662,0.00736560038765615,
-1.78170078744151));
#22752=CARTESIAN_POINT('Ctrl Pts',(93.6163760857269,0.173059326225834,-1.76800253109418));
#22753=CARTESIAN_POINT('Ctrl Pts',(93.6181137572511,0.199716908733858,-1.76518993772296));
#22754=CARTESIAN_POINT('Ctrl Pts',(93.6209359564715,0.242435528103644,-1.75970274251314));
#22755=CARTESIAN_POINT('Ctrl Pts',(93.6220086385425,0.258541777319047,-1.75740856018637));
#22756=CARTESIAN_POINT('Ctrl Pts',(93.6239280788793,0.287114737630044,-1.75293733199359));
#22757=CARTESIAN_POINT('Ctrl Pts',(93.6247720183785,0.299594121137149,-1.75084765494246));
#22758=CARTESIAN_POINT('Ctrl Pts',(93.6265673228836,0.32595791259679,-1.74614291976344));
#22759=CARTESIAN_POINT('Ctrl Pts',(93.6275196752413,0.339835514082865,-1.74349518504779));
#22760=CARTESIAN_POINT('Ctrl Pts',(93.6301053351699,0.377214501751471,-1.73590035285499));
#22761=CARTESIAN_POINT('Ctrl Pts',(93.6317484378353,0.400648825719022,-1.73064185643832));
#22762=CARTESIAN_POINT('Ctrl Pts',(93.6354372238,0.452531851930095,-1.71788944563346));
#22763=CARTESIAN_POINT('Ctrl Pts',(93.6374898119668,0.480915020752726,-1.71016075126501));
#22764=CARTESIAN_POINT('Ctrl Pts',(93.6442070844146,0.572235747237687,-1.68284113952823));
#22765=CARTESIAN_POINT('Ctrl Pts',(93.6489494740752,0.634273448957008,-1.66045287928878));
#22766=CARTESIAN_POINT('Ctrl Pts',(93.6609455689353,0.786037517344467,-1.5959361436853));
#22767=CARTESIAN_POINT('Ctrl Pts',(93.6682500317492,0.873758085446539,-1.54964977862052));
#22768=CARTESIAN_POINT('Ctrl Pts',(93.6781763639195,0.990238545375748,-1.47513833322026));
#22769=CARTESIAN_POINT('Ctrl Pts',(93.6809596625256,1.02260385476284,-1.45288931172616));
#22770=CARTESIAN_POINT('Ctrl Pts',(93.6845254577908,1.06397539720641,-1.42238100028658));
#22771=CARTESIAN_POINT('Ctrl Pts',(93.6853615654813,1.07366947045865,-1.41507782280452));
#22772=CARTESIAN_POINT('Ctrl Pts',(93.6867106462214,1.08931179493333,-1.40304014426578));
#22773=CARTESIAN_POINT('Ctrl Pts',(93.687227575559,1.09530566104463,-1.39836595617888));
#22774=CARTESIAN_POINT('Ctrl Pts',(93.6882474037055,1.10713462570381,-1.38901866907892));
#22775=CARTESIAN_POINT('Ctrl Pts',(93.6887503698382,1.1129705645062,-1.38434694684716));
#22776=CARTESIAN_POINT('Ctrl Pts',(93.6900241067932,1.12774915105447,-1.37236268954325));
#22777=CARTESIAN_POINT('Ctrl Pts',(93.6907913461591,1.13665046274147,-1.36499935623864));
#22778=CARTESIAN_POINT('Ctrl Pts',(93.6939978552124,1.17381288887357,-1.33364226613764));
#22779=CARTESIAN_POINT('Ctrl Pts',(93.6963858510205,1.20139313028419,-1.30885193374254));
#22780=CARTESIAN_POINT('Ctrl Pts',(93.7032746749132,1.27985350078847,-1.23375661584138));
#22781=CARTESIAN_POINT('Ctrl Pts',(93.7076721859276,1.32849666361159,-1.181219021491));
#22782=CARTESIAN_POINT('Ctrl Pts',(93.719491892003,1.45052343439877,-1.0323183553378));
#22783=CARTESIAN_POINT('Ctrl Pts',(93.7268930778586,1.51743747596037,-0.931170761123306));
#22784=CARTESIAN_POINT('Ctrl Pts',(93.736253958162,1.58483166639567,-0.802473594830802));
#22785=CARTESIAN_POINT('Ctrl Pts',(93.7378344106899,1.59566760071422,-0.780704872442546));
#22786=CARTESIAN_POINT('Ctrl Pts',(93.7404512344874,1.61269830521266,-0.744654469483821));
#22787=CARTESIAN_POINT('Ctrl Pts',(93.7414784508323,1.61915843455582,-0.730501225633464));
#22788=CARTESIAN_POINT('Ctrl Pts',(93.7433486220229,1.63050890130123,-0.704743440816549));
#22789=CARTESIAN_POINT('Ctrl Pts',(93.7441893135793,1.63546338126657,-0.693168167969974));
#22790=CARTESIAN_POINT('Ctrl Pts',(93.7460136170739,1.64589405277667,-0.668064235254204));
#22791=CARTESIAN_POINT('Ctrl Pts',(93.7469986104917,1.65132736618654,-0.654518878940241));
#22792=CARTESIAN_POINT('Ctrl Pts',(93.7497725941038,1.66607201194726,-0.616407543386504));
#22793=CARTESIAN_POINT('Ctrl Pts',(93.7515739676873,1.67500582486124,-0.591700571709546));
#22794=CARTESIAN_POINT('Ctrl Pts',(93.7594892978949,1.71148069428218,-0.483371806523794));
#22795=CARTESIAN_POINT('Ctrl Pts',(93.7657814445003,1.73332768841504,-0.397976869663198));
#22796=CARTESIAN_POINT('Ctrl Pts',(93.7764962663586,1.75916937453405,-0.252820987874083));
#22797=CARTESIAN_POINT('Ctrl Pts',(93.7808533281167,1.76664216406746,-0.193831279908814));
#22798=CARTESIAN_POINT('Ctrl Pts',(93.7873138516248,1.77334623387469,-0.105601855031709));
#22799=CARTESIAN_POINT('Ctrl Pts',(93.7894295803521,1.77483613273508,-0.0765806551991079));
#22800=CARTESIAN_POINT('Ctrl Pts',(93.79153079842,1.7756136390086,-0.0475422703142009));
#22801=CARTESIAN_POINT('Origin',(88.3562164250559,0.,0.));
#22802=CARTESIAN_POINT('',(94.6900676319114,1.77561363837122,-0.0475422941192622));
#22803=CARTESIAN_POINT('',(94.5412649413994,1.77561364082572,-0.0475422024484503));
#22804=CARTESIAN_POINT('',(88.3562164250559,1.77561363837197,-0.0475422940912398));
#22805=CARTESIAN_POINT('Ctrl Pts',(94.6900676319114,1.77561363837047,-0.0475422941472846));
#22806=CARTESIAN_POINT('Ctrl Pts',(94.6893374515194,1.77532329368649,-0.0583861120561661));
#22807=CARTESIAN_POINT('Ctrl Pts',(94.6886041642756,1.77493362258899,-0.0692269101151485));
#22808=CARTESIAN_POINT('Ctrl Pts',(94.6861231269635,1.77328633428699,-0.105735780798001));
#22809=CARTESIAN_POINT('Ctrl Pts',(94.6843612362446,1.77157104388246,-0.131378821437202));
#22810=CARTESIAN_POINT('Ctrl Pts',(94.6732661564457,1.75740653431339,-0.291030668250471));
#22811=CARTESIAN_POINT('Ctrl Pts',(94.6634727861833,1.73031769151216,-0.423278290624867));
#22812=CARTESIAN_POINT('Ctrl Pts',(94.6490381426011,1.66906605814486,-0.610928612591884));
#22813=CARTESIAN_POINT('Ctrl Pts',(94.6444502734985,1.6464015994563,-0.669610258070475));
#22814=CARTESIAN_POINT('Ctrl Pts',(94.6374965125478,1.60658286213221,-0.758380334676792));
#22815=CARTESIAN_POINT('Ctrl Pts',(94.6350661121503,1.5915818465348,-0.789377488560802));
#22816=CARTESIAN_POINT('Ctrl Pts',(94.6318978470677,1.57045723920818,-0.829973818142713));
#22817=CARTESIAN_POINT('Ctrl Pts',(94.6311184460216,1.56513006046956,-0.839976422134724));
#22818=CARTESIAN_POINT('Ctrl Pts',(94.6298340962298,1.5561277531675,-0.856496609803153));
#22819=CARTESIAN_POINT('Ctrl Pts',(94.6293259141241,1.55250658654819,-0.863043065485869));
#22820=CARTESIAN_POINT('Ctrl Pts',(94.6282952337822,1.54503884003291,-0.87634437415588));
#22821=CARTESIAN_POINT('Ctrl Pts',(94.6277729419677,1.54118909821517,-0.883097190977505));
#22822=CARTESIAN_POINT('Ctrl Pts',(94.626404267074,1.53093162946895,-0.900818385219357));
#22823=CARTESIAN_POINT('Ctrl Pts',(94.6255624403535,1.5244502259585,-0.911743905312175));
#22824=CARTESIAN_POINT('Ctrl Pts',(94.6217892606524,1.49464841198525,-0.960773575382697));
#22825=CARTESIAN_POINT('Ctrl Pts',(94.6189322313152,1.47001083714337,-0.998062424214972));
#22826=CARTESIAN_POINT('Ctrl Pts',(94.6101405256078,1.38866051089384,-1.11162659655119));
#22827=CARTESIAN_POINT('Ctrl Pts',(94.6043726783083,1.32721869853184,-1.18430749471312));
#22828=CARTESIAN_POINT('Ctrl Pts',(94.5930713966691,1.19785774846736,-1.31454968153972));
#22829=CARTESIAN_POINT('Ctrl Pts',(94.5875642335257,1.13085765647851,-1.37261154852834));
#22830=CARTESIAN_POINT('Ctrl Pts',(94.5801508325271,1.03859273067365,-1.44121075572246));
#22831=CARTESIAN_POINT('Ctrl Pts',(94.5784295087121,1.01702350042697,-1.45651171768604));
#22832=CARTESIAN_POINT('Ctrl Pts',(94.5757215184839,0.982928583068523,-1.47957160759876));
#22833=CARTESIAN_POINT('Ctrl Pts',(94.5747475580119,0.970633798589597,-1.48766620870782));
#22834=CARTESIAN_POINT('Ctrl Pts',(94.5729211758183,0.947529175157864,-1.50246941530146));
#22835=CARTESIAN_POINT('Ctrl Pts',(94.5720702623001,0.936745052639939,-1.50921654294944));
#22836=CARTESIAN_POINT('Ctrl Pts',(94.5701560688634,0.912448093814269,-1.52405728910833));
#22837=CARTESIAN_POINT('Ctrl Pts',(94.5690905733052,0.898898343640544,-1.53208807980124));
#22838=CARTESIAN_POINT('Ctrl Pts',(94.5663374345393,0.863833107380073,-1.55224558014611));
#22839=CARTESIAN_POINT('Ctrl Pts',(94.5646404701187,0.842168879709873,-1.56410531932907));
#22840=CARTESIAN_POINT('Ctrl Pts',(94.5556614541638,0.72732008628012,-1.62389963563221));
#22841=CARTESIAN_POINT('Ctrl Pts',(94.548115758263,0.630289607248745,-1.66396308995811));
#22842=CARTESIAN_POINT('Ctrl Pts',(94.5344082194848,0.451082534983792,-1.72002321734563));
#22843=CARTESIAN_POINT('Ctrl Pts',(94.5283057451115,0.370213076920247,-1.73922350816295));
#22844=CARTESIAN_POINT('Ctrl Pts',(94.5203841746582,0.261368930872614,-1.75712691441568));
#22845=CARTESIAN_POINT('Ctrl Pts',(94.5184412413556,0.234342525185479,-1.76093510727185));
#22846=CARTESIAN_POINT('Ctrl Pts',(94.5151506770191,0.187845216956855,-1.76639732115271));
#22847=CARTESIAN_POINT('Ctrl Pts',(94.5137911805211,0.168415447642005,-1.76835563079447));
#22848=CARTESIAN_POINT('Ctrl Pts',(94.5118173957431,0.139827634018304,-1.77076148006389));
#22849=CARTESIAN_POINT('Ctrl Pts',(94.5111906683815,0.130692836792508,-1.77145910994884));
#22850=CARTESIAN_POINT('Ctrl Pts',(94.5100800024859,0.114394418493414,-1.77257706829787));
#22851=CARTESIAN_POINT('Ctrl Pts',(94.5095946261354,0.107233180361402,-1.77302470270061));
#22852=CARTESIAN_POINT('Ctrl Pts',(94.5085141801711,0.0912056668894408,
-1.77392908473936));
#22853=CARTESIAN_POINT('Ctrl Pts',(94.5079203775127,0.0823384688998834,
-1.77436277472453));
#22854=CARTESIAN_POINT('Ctrl Pts',(94.5061314426169,0.0554608507568541,
-1.77547542232024));
#22855=CARTESIAN_POINT('Ctrl Pts',(94.5049470565469,0.0374423872332112,
-1.77594679264801));
#22856=CARTESIAN_POINT('Ctrl Pts',(94.4976226473424,-0.0751355753381771,
-1.77717763609404));
#22857=CARTESIAN_POINT('Ctrl Pts',(94.4918022655074,-0.169634026652738,
-1.77065932009031));
#22858=CARTESIAN_POINT('Ctrl Pts',(94.4782464675659,-0.387937841560564,
-1.73795389651269));
#22859=CARTESIAN_POINT('Ctrl Pts',(94.4705389267968,-0.510341176426477,
-1.70602670806349));
#22860=CARTESIAN_POINT('Ctrl Pts',(94.4607475474385,-0.652208696669796,
-1.65237401569988));
#22861=CARTESIAN_POINT('Ctrl Pts',(94.4590838711563,-0.675893644146779,
-1.64282797224383));
#22862=CARTESIAN_POINT('Ctrl Pts',(94.4564465028495,-0.712723212967857,
-1.62705282831613));
#22863=CARTESIAN_POINT('Ctrl Pts',(94.4554844293663,-0.726011681660081,
-1.62116695666736));
#22864=CARTESIAN_POINT('Ctrl Pts',(94.4536684694263,-0.750810297153695,
-1.60981684200193));
#22865=CARTESIAN_POINT('Ctrl Pts',(94.4528159340303,-0.762336845134641,
-1.6043905032895));
#22866=CARTESIAN_POINT('Ctrl Pts',(94.4508820805722,-0.788216608979539,
-1.59186526668863));
#22867=CARTESIAN_POINT('Ctrl Pts',(94.4497983416878,-0.802534038311092,
-1.58469540857963));
#22868=CARTESIAN_POINT('Ctrl Pts',(94.4464517788779,-0.846165971533108,
-1.56210254280354));
#22869=CARTESIAN_POINT('Ctrl Pts',(94.4441672037941,-0.875146139580199,
-1.54605309898268));
#22870=CARTESIAN_POINT('Ctrl Pts',(94.4323924040923,-1.02037565184145,-1.46023198679797));
#22871=CARTESIAN_POINT('Ctrl Pts',(94.4224632205585,-1.1287959833686,-1.37813351488065));
#22872=CARTESIAN_POINT('Ctrl Pts',(94.4072430933574,-1.27952273879188,-1.23417966700966));
#22873=CARTESIAN_POINT('Ctrl Pts',(94.4019540389607,-1.32909471514766,-1.18062998039253));
#22874=CARTESIAN_POINT('Ctrl Pts',(94.3955873617998,-1.38656557139963,-1.11032439354308));
#22875=CARTESIAN_POINT('Ctrl Pts',(94.3943437695617,-1.39768260143938,-1.09629729073699));
#22876=CARTESIAN_POINT('Ctrl Pts',(94.3925053278173,-1.41397953445161,-1.07508339852437));
#22877=CARTESIAN_POINT('Ctrl Pts',(94.3919002584852,-1.41932041220726,-1.06802247802508));
#22878=CARTESIAN_POINT('Ctrl Pts',(94.3908600475587,-1.42846633488624,-1.05574130965536));
#22879=CARTESIAN_POINT('Ctrl Pts',(94.3904232530224,-1.43229592600246,-1.05053994056219));
#22880=CARTESIAN_POINT('Ctrl Pts',(94.3893954280319,-1.44128126104364,-1.03819554296366));
#22881=CARTESIAN_POINT('Ctrl Pts',(94.3888060740894,-1.44641234559371,-1.03103491387593));
#22882=CARTESIAN_POINT('Ctrl Pts',(94.3870446909205,-1.46167506337268,-1.00939699652882));
#22883=CARTESIAN_POINT('Ctrl Pts',(94.3858829284997,-1.47164449465209,-0.994805924285774));
#22884=CARTESIAN_POINT('Ctrl Pts',(94.3778842867471,-1.53944013882501,-0.892331255709796));
#22885=CARTESIAN_POINT('Ctrl Pts',(94.3714481301101,-1.58958400814105,-0.799599560930391));
#22886=CARTESIAN_POINT('Ctrl Pts',(94.3600092359002,-1.66333984383855,-0.628449063888252));
#22887=CARTESIAN_POINT('Ctrl Pts',(94.3550301136434,-1.69030649370887,-0.551824689823842));
#22888=CARTESIAN_POINT('Ctrl Pts',(94.3468206407555,-1.72502387187582,-0.42633832116108));
#22889=CARTESIAN_POINT('Ctrl Pts',(94.3436817704253,-1.73614141110801,-0.378528810246688));
#22890=CARTESIAN_POINT('Ctrl Pts',(94.3392747009371,-1.7487020001742,-0.312164897040442));
#22891=CARTESIAN_POINT('Ctrl Pts',(94.3380603739705,-1.75185512837645,-0.293954376083439));
#22892=CARTESIAN_POINT('Ctrl Pts',(94.3359702840145,-1.75675580004252,-0.262763336384444));
#22893=CARTESIAN_POINT('Ctrl Pts',(94.3350990659994,-1.75864500923082,-0.249806380547978));
#22894=CARTESIAN_POINT('Ctrl Pts',(94.3333215322251,-1.76218828575521,-0.223468708354198));
#22895=CARTESIAN_POINT('Ctrl Pts',(94.3324150010505,-1.76383359686637,-0.210087703592546));
#22896=CARTESIAN_POINT('Ctrl Pts',(94.3301191666405,-1.76759409278264,-0.176336537589576));
#22897=CARTESIAN_POINT('Ctrl Pts',(94.3287236932569,-1.76950955184938,-0.155946580303943));
#22898=CARTESIAN_POINT('Ctrl Pts',(94.3230276537799,-1.77583743956784,-0.073254593266782));
#22899=CARTESIAN_POINT('Ctrl Pts',(94.3186379483455,-1.77731456176376,-0.0107795545668774));
#22900=CARTESIAN_POINT('Ctrl Pts',(94.3043426769924,-1.77150701968772,0.18890634582484));
#22901=CARTESIAN_POINT('Ctrl Pts',(94.2941433169928,-1.75161086856034,0.325233890425397));
#22902=CARTESIAN_POINT('Ctrl Pts',(94.2813585991203,-1.7057481420427,0.49712727467627));
#22903=CARTESIAN_POINT('Ctrl Pts',(94.2784776287621,-1.69393969129844,0.535986135145742));
#22904=CARTESIAN_POINT('Ctrl Pts',(94.274803909654,-1.67681993706431,0.586081143204528));
#22905=CARTESIAN_POINT('Ctrl Pts',(94.2739538902563,-1.67270948431136,0.597711644840104));
#22906=CARTESIAN_POINT('Ctrl Pts',(94.2725846952867,-1.6658391543421,0.616525066251105));
#22907=CARTESIAN_POINT('Ctrl Pts',(94.2720614174575,-1.66315326214235,0.623734300639063));
#22908=CARTESIAN_POINT('Ctrl Pts',(94.2710306852491,-1.65774122754958,0.637977259474338));
#22909=CARTESIAN_POINT('Ctrl Pts',(94.2705231476407,-1.65501696665022,0.64501147694608));
#22910=CARTESIAN_POINT('Ctrl Pts',(94.2692393470779,-1.64797710019312,0.662850588400758));
#22911=CARTESIAN_POINT('Ctrl Pts',(94.2684666560659,-1.64359990349287,0.673631056693287));
#22912=CARTESIAN_POINT('Ctrl Pts',(94.2652467297818,-1.62478474101254,0.718694893084872));
#22913=CARTESIAN_POINT('Ctrl Pts',(94.2628510300613,-1.60937655816748,0.752565842649512));
#22914=CARTESIAN_POINT('Ctrl Pts',(94.2559421657426,-1.5611726968115,0.850264866256651));
#22915=CARTESIAN_POINT('Ctrl Pts',(94.2515325657993,-1.52556009584107,0.91262167407638));
#22916=CARTESIAN_POINT('Ctrl Pts',(94.2397399594445,-1.42037917791901,1.0733436565479));
#22917=CARTESIAN_POINT('Ctrl Pts',(94.2323765982472,-1.34443429641627,1.16706303439117));
#22918=CARTESIAN_POINT('Ctrl Pts',(94.2230516045925,-1.24238243993935,1.26970331890244));
#22919=CARTESIAN_POINT('Ctrl Pts',(94.2214641821524,-1.22480632970158,1.2866662377068));
#22920=CARTESIAN_POINT('Ctrl Pts',(94.2188328325687,-1.19538807113728,1.31390906364636));
#22921=CARTESIAN_POINT('Ctrl Pts',(94.2177981081761,-1.18374933191899,1.32440445523666));
#22922=CARTESIAN_POINT('Ctrl Pts',(94.2159119952549,-1.16241806197842,1.34313439925979));
#22923=CARTESIAN_POINT('Ctrl Pts',(94.2150628822803,-1.15277297514628,1.35142155473046));
#22924=CARTESIAN_POINT('Ctrl Pts',(94.2132174362284,-1.13172616754371,1.36911592562504));
#22925=CARTESIAN_POINT('Ctrl Pts',(94.2122196625026,-1.12029440772412,1.37848574641721));
#22926=CARTESIAN_POINT('Ctrl Pts',(94.209400296511,-1.08785505707932,1.40440398805559));
#22927=CARTESIAN_POINT('Ctrl Pts',(94.207565819018,-1.0665895317994,1.42062163221472));
#22928=CARTESIAN_POINT('Ctrl Pts',(94.1994189944927,-0.97151033826795,1.48979311437445));
#22929=CARTESIAN_POINT('Ctrl Pts',(94.1929165196412,-0.894073161718743,
1.53751250252177));
#22930=CARTESIAN_POINT('Ctrl Pts',(94.1790751612384,-0.724933105126678,
1.62463065929377));
#22931=CARTESIAN_POINT('Ctrl Pts',(94.1717385091288,-0.632860841533863,
1.66266065870763));
#22932=CARTESIAN_POINT('Ctrl Pts',(94.1618360132447,-0.501338220428661,
1.70446799208706));
#22933=CARTESIAN_POINT('Ctrl Pts',(94.159103355935,-0.46421365473568,1.71495111383151));
#22934=CARTESIAN_POINT('Ctrl Pts',(94.1555859666233,-0.414989972006551,
1.72713484271013));
#22935=CARTESIAN_POINT('Ctrl Pts',(94.1547496703116,-0.403175594999771,
1.72993089513585));
#22936=CARTESIAN_POINT('Ctrl Pts',(94.1533970134952,-0.383870142125925,
1.73429129995688));
#22937=CARTESIAN_POINT('Ctrl Pts',(94.1528767248285,-0.37639621702699,1.73592871183059));
#22938=CARTESIAN_POINT('Ctrl Pts',(94.1518465497956,-0.361496740912076,
1.73909218561173));
#22939=CARTESIAN_POINT('Ctrl Pts',(94.1513366301004,-0.354071556981567,
1.74061910282712));
#22940=CARTESIAN_POINT('Ctrl Pts',(94.1500388449784,-0.335052546802409,
1.74440343904303));
#22941=CARTESIAN_POINT('Ctrl Pts',(94.1492547100042,-0.32344533206813,1.74659288421936));
#22942=CARTESIAN_POINT('Ctrl Pts',(94.1459102440446,-0.273487489281059,
1.75550121107037));
#22943=CARTESIAN_POINT('Ctrl Pts',(94.1434065570145,-0.234940588370822,
1.76107448358309));
#22944=CARTESIAN_POINT('Ctrl Pts',(94.1360132952326,-0.118868961974354,
1.77397696013767));
#22945=CARTESIAN_POINT('Ctrl Pts',(94.1312450137954,-0.0410124122563852,
1.77748239804443));
#22946=CARTESIAN_POINT('Ctrl Pts',(94.1196087017441,0.148528879026554,1.7735517576253));
#22947=CARTESIAN_POINT('Ctrl Pts',(94.1127431696131,0.259750139340181,1.76070238192323));
#22948=CARTESIAN_POINT('Ctrl Pts',(94.1039620375275,0.393111428559367,1.73237811811083));
#22949=CARTESIAN_POINT('Ctrl Pts',(94.1023618566181,0.417090846235809,1.72676161371742));
#22950=CARTESIAN_POINT('Ctrl Pts',(94.0997137961818,0.456182855686057,1.71674363561967));
#22951=CARTESIAN_POINT('Ctrl Pts',(94.0986753269721,0.471367889458472,1.71263650389831));
#22952=CARTESIAN_POINT('Ctrl Pts',(94.096785279977,0.498729181589673,1.70484458349575));
#22953=CARTESIAN_POINT('Ctrl Pts',(94.0959360240724,0.510924333149826,1.70122960289306));
#22954=CARTESIAN_POINT('Ctrl Pts',(94.0940935758403,0.53716131431373,1.69314468279882));
#22955=CARTESIAN_POINT('Ctrl Pts',(94.0930989804083,0.551188360896928,1.6886303806519));
#22956=CARTESIAN_POINT('Ctrl Pts',(94.0902982139475,0.590297733114425,1.6755046655299));
#22957=CARTESIAN_POINT('Ctrl Pts',(94.0884794302712,0.615244844818676,1.66650560952092));
#22958=CARTESIAN_POINT('Ctrl Pts',(94.0804693826694,0.723115473339314,1.62484172722915));
#22959=CARTESIAN_POINT('Ctrl Pts',(94.0740955019575,0.803704434977019,1.58652503101406));
#22960=CARTESIAN_POINT('Ctrl Pts',(94.0606279868053,0.964542411749395,1.49464501365388));
#22961=CARTESIAN_POINT('Ctrl Pts',(94.0535384469619,1.04400664639059,1.44026251287449));
#22962=CARTESIAN_POINT('Ctrl Pts',(94.0435125864332,1.15218511719984,1.35255095345306));
#22963=CARTESIAN_POINT('Ctrl Pts',(94.0404463695849,1.1846924336517,1.324171107772));
#22964=CARTESIAN_POINT('Ctrl Pts',(94.0365790225439,1.22529120948223,1.28603392999653));
#22965=CARTESIAN_POINT('Ctrl Pts',(94.0357131195092,1.23435455506811,1.27733733687547));
#22966=CARTESIAN_POINT('Ctrl Pts',(94.0343247823576,1.24885424043248,1.26312591835201));
#22967=CARTESIAN_POINT('Ctrl Pts',(94.033798041286,1.25434791947277,1.25767058572045));
#22968=CARTESIAN_POINT('Ctrl Pts',(94.032766406138,1.26509582218615,1.24685722195689));
#22969=CARTESIAN_POINT('Ctrl Pts',(94.0322613727069,1.27035205677732,1.24150152099397));
#22970=CARTESIAN_POINT('Ctrl Pts',(94.0309925414292,1.28353883052675,1.22789377224332));
#22971=CARTESIAN_POINT('Ctrl Pts',(94.0302321473457,1.29142402201694,1.21959790829906));
#22972=CARTESIAN_POINT('Ctrl Pts',(94.0271397083271,1.32338960725514,1.18530983810032));
#22973=CARTESIAN_POINT('Ctrl Pts',(94.0248542374336,1.34677155586203,1.15867434406262));
#22974=CARTESIAN_POINT('Ctrl Pts',(94.0184116380934,1.41135837396323,1.08050128714177));
#22975=CARTESIAN_POINT('Ctrl Pts',(94.0143423418909,1.45051148641425,1.02734274289743));
#22976=CARTESIAN_POINT('Ctrl Pts',(94.0023456079645,1.55736036323134,0.8639446436584));
#22977=CARTESIAN_POINT('Ctrl Pts',(93.9944693107659,1.61607519881808,0.748377282910658));
#22978=CARTESIAN_POINT('Ctrl Pts',(93.9844457045107,1.67099695358711,0.602927308744723));
#22979=CARTESIAN_POINT('Ctrl Pts',(93.9827385154483,1.67971820255529,0.578185785918303));
#22980=CARTESIAN_POINT('Ctrl Pts',(93.9800380918145,1.69250697331467,0.539169833474381));
#22981=CARTESIAN_POINT('Ctrl Pts',(93.9790571772064,1.69694912515043,0.525021531269705));
#22982=CARTESIAN_POINT('Ctrl Pts',(93.9772244569097,1.7048695849922,0.498643544495678));
#22983=CARTESIAN_POINT('Ctrl Pts',(93.9763742497931,1.70839475732654,0.486428848790857));
#22984=CARTESIAN_POINT('Ctrl Pts',(93.9744703683221,1.71595596094587,0.45913278932863));
#22985=CARTESIAN_POINT('Ctrl Pts',(93.973414587813,1.71992484600809,0.444034092207501));
#22986=CARTESIAN_POINT('Ctrl Pts',(93.9702452912737,1.73117074183514,0.398836746340757));
#22987=CARTESIAN_POINT('Ctrl Pts',(93.9681132561072,1.73785993092249,0.368599428804067));
#22988=CARTESIAN_POINT('Ctrl Pts',(93.9630964330432,1.75157728904911,0.297873799108614));
#22989=CARTESIAN_POINT('Ctrl Pts',(93.9601947148737,1.75799738984498,0.257286882321925));
#22990=CARTESIAN_POINT('Ctrl Pts',(93.9513094686424,1.77315323233064,0.133879078515832));
#22991=CARTESIAN_POINT('Ctrl Pts',(93.9452264076527,1.7774785525948,0.0506361430331844));
#22992=CARTESIAN_POINT('Ctrl Pts',(93.9387739566831,1.77585943002973,-0.037579036994388));
#22993=CARTESIAN_POINT('Ctrl Pts',(93.9384095511236,1.77574701040699,-0.0425611044426868));
#22994=CARTESIAN_POINT('Ctrl Pts',(93.9380452419004,1.77561363825831,-0.0475422983361156));
#22995=CARTESIAN_POINT('Ctrl Pts',(93.79153079842,1.7756136390086,-0.0475422703142009));
#22996=CARTESIAN_POINT('Ctrl Pts',(93.7951001279053,1.776934385346,0.00178510077781863));
#22997=CARTESIAN_POINT('Ctrl Pts',(93.7986279292612,1.77619947883391,0.0511620355513193));
#22998=CARTESIAN_POINT('Ctrl Pts',(93.8030481184526,1.77261024993695,0.114522261575697));
#22999=CARTESIAN_POINT('Ctrl Pts',(93.8040216851538,1.77164638042591,0.128575194345392));
#23000=CARTESIAN_POINT('Ctrl Pts',(93.8055361665494,1.76987129544117,0.15061214357101));
#23001=CARTESIAN_POINT('Ctrl Pts',(93.8060829002402,1.76917299833563,0.158604314502194));
#23002=CARTESIAN_POINT('Ctrl Pts',(93.8071166449974,1.76774236346225,0.173790932308062));
#23003=CARTESIAN_POINT('Ctrl Pts',(93.8076041625932,1.76702021329073,0.180985964401413));
#23004=CARTESIAN_POINT('Ctrl Pts',(93.8087779001014,1.76516666704678,0.1983836380883));
#23005=CARTESIAN_POINT('Ctrl Pts',(93.8094616817121,1.76399070989842,0.208581442973571));
#23006=CARTESIAN_POINT('Ctrl Pts',(93.8119028513006,1.7594476584015,0.245187015983037));
#23007=CARTESIAN_POINT('Ctrl Pts',(93.8136347086749,1.75557524059647,0.27152990863758));
#23008=CARTESIAN_POINT('Ctrl Pts',(93.8180595208785,1.74402280435814,0.339465238934993));
#23009=CARTESIAN_POINT('Ctrl Pts',(93.8207171867516,1.73544689433007,0.38088939307791));
#23010=CARTESIAN_POINT('Ctrl Pts',(93.828377690126,1.70617817965795,0.500566599623081));
#23011=CARTESIAN_POINT('Ctrl Pts',(93.8332999765335,1.68160813585582,0.577759152340324));
#23012=CARTESIAN_POINT('Ctrl Pts',(93.8439103356994,1.61832881858997,0.737831319096879));
#23013=CARTESIAN_POINT('Ctrl Pts',(93.8496033183079,1.57831793249048,0.819934583248301));
#23014=CARTESIAN_POINT('Ctrl Pts',(93.8569583208778,1.5209413323599,0.917766519669438));
#23015=CARTESIAN_POINT('Ctrl Pts',(93.8584113577249,1.50934052661553,0.93672249030981));
#23016=CARTESIAN_POINT('Ctrl Pts',(93.8607845531922,1.48999031214843,0.96704811037777));
#23017=CARTESIAN_POINT('Ctrl Pts',(93.8616966430971,1.48245887022327,0.978554473786703));
#23018=CARTESIAN_POINT('Ctrl Pts',(93.8634645017353,1.46768517412862,1.00056334926166));
#23019=CARTESIAN_POINT('Ctrl Pts',(93.8643195170617,1.46046186628465,1.0110775977473));
#23020=CARTESIAN_POINT('Ctrl Pts',(93.8663277947901,1.44331841241669,1.03546456360478));
#23021=CARTESIAN_POINT('Ctrl Pts',(93.8674843711257,1.43331061953878,1.04927381295778));
#23022=CARTESIAN_POINT('Ctrl Pts',(93.871369080488,1.39926088745102,1.09486108613009));
#23023=CARTESIAN_POINT('Ctrl Pts',(93.874130672568,1.37435023564364,1.12597194470871));
#23024=CARTESIAN_POINT('Ctrl Pts',(93.881055981465,1.31019680618218,1.20078967825894));
#23025=CARTESIAN_POINT('Ctrl Pts',(93.8852609356911,1.26979416025413,1.24343604478015));
#23026=CARTESIAN_POINT('Ctrl Pts',(93.8977286388729,1.14543270153583,1.36231136470535));
#23027=CARTESIAN_POINT('Ctrl Pts',(93.9061144470148,1.05620323854568,1.43260002810284));
#23028=CARTESIAN_POINT('Ctrl Pts',(93.9168910441379,0.929728499158324,1.51394894381923));
#23029=CARTESIAN_POINT('Ctrl Pts',(93.9195131425905,0.89794894028685,1.53301162139284));
#23030=CARTESIAN_POINT('Ctrl Pts',(93.9229074179601,0.85519821914223,1.55686922931175));
#23031=CARTESIAN_POINT('Ctrl Pts',(93.9237272219086,0.844744052007549,1.56256625371961));
#23032=CARTESIAN_POINT('Ctrl Pts',(93.9250055828191,0.82822680827509,1.57135314324666));
#23033=CARTESIAN_POINT('Ctrl Pts',(93.9254683719418,0.822202137801622,1.57451389173938));
#23034=CARTESIAN_POINT('Ctrl Pts',(93.9264267841305,0.809627984207273,1.58101886921314));
#23035=CARTESIAN_POINT('Ctrl Pts',(93.9269219914552,0.80307566624127,1.58435716124668));
#23036=CARTESIAN_POINT('Ctrl Pts',(93.928148429081,0.786715607287767,1.59256475902223));
#23037=CARTESIAN_POINT('Ctrl Pts',(93.928876650081,0.776883001163696,1.59738435452997));
#23038=CARTESIAN_POINT('Ctrl Pts',(93.9316973292596,0.738364944915256,1.61582474439925));
#23039=CARTESIAN_POINT('Ctrl Pts',(93.9337526791903,0.709359084570396,1.62876713468873));
#23040=CARTESIAN_POINT('Ctrl Pts',(93.9393072948116,0.628930376417344,1.66209777837205));
#23041=CARTESIAN_POINT('Ctrl Pts',(93.9427447310023,0.5768764502547,1.68087383304231));
#23042=CARTESIAN_POINT('Ctrl Pts',(93.9547875890271,0.390278508504457,1.73848816636115));
#23043=CARTESIAN_POINT('Ctrl Pts',(93.9632476708782,0.252128709187763,1.76382727580857));
#23044=CARTESIAN_POINT('Ctrl Pts',(93.9739386976448,0.0860788704251266,
1.77435965566323));
#23045=CARTESIAN_POINT('Ctrl Pts',(93.9756518002809,0.0596850399432994,
1.77544342066861));
#23046=CARTESIAN_POINT('Ctrl Pts',(93.9784419853642,0.0171217143288013,
1.77624098129434));
#23047=CARTESIAN_POINT('Ctrl Pts',(93.9795076633116,0.000962604192458216,
1.77632323112394));
#23048=CARTESIAN_POINT('Ctrl Pts',(93.981419351571,-0.0278356676466562,
1.77607686704211));
#23049=CARTESIAN_POINT('Ctrl Pts',(93.9822626288065,-0.0404745851562134,
1.77583379171689));
#23050=CARTESIAN_POINT('Ctrl Pts',(93.9840616042502,-0.0672936444328707,
1.77503154797161));
#23051=CARTESIAN_POINT('Ctrl Pts',(93.9850183444686,-0.0814717671662096,
1.77443730845902));
#23052=CARTESIAN_POINT('Ctrl Pts',(93.987629098197,-0.119921299439404,1.77236401355179));
#23053=CARTESIAN_POINT('Ctrl Pts',(93.9892932365374,-0.14417114574734,1.77055637951881));
#23054=CARTESIAN_POINT('Ctrl Pts',(93.9930373361706,-0.198133422439832,
1.76541802088226));
#23055=CARTESIAN_POINT('Ctrl Pts',(93.9951245279484,-0.227813734626224,
1.76183380705522));
#23056=CARTESIAN_POINT('Ctrl Pts',(94.0020064016542,-0.324374436079653,
1.74769239432223));
#23057=CARTESIAN_POINT('Ctrl Pts',(94.0068831034637,-0.390738935228149,
1.73406141429018));
#23058=CARTESIAN_POINT('Ctrl Pts',(94.0193503432439,-0.556247636455101,
1.69008221509953));
#23059=CARTESIAN_POINT('Ctrl Pts',(94.026994284601,-0.653820697743124,1.65478362061564));
#23060=CARTESIAN_POINT('Ctrl Pts',(94.0367697288277,-0.777951948391084,
1.59717326568779));
#23061=CARTESIAN_POINT('Ctrl Pts',(94.0391185229558,-0.807742611733825,
1.58231598681615));
#23062=CARTESIAN_POINT('Ctrl Pts',(94.0422175355942,-0.847207640106647,
1.56122855573939));
#23063=CARTESIAN_POINT('Ctrl Pts',(94.0430059930102,-0.857262840544182,
1.55572999855696));
#23064=CARTESIAN_POINT('Ctrl Pts',(94.0442473189012,-0.873127108806972,
1.54685430590564));
#23065=CARTESIAN_POINT('Ctrl Pts',(94.0447040278569,-0.878971238317084,
1.54354098029815));
#23066=CARTESIAN_POINT('Ctrl Pts',(94.0456616317238,-0.891243343935174,
1.53649101571774));
#23067=CARTESIAN_POINT('Ctrl Pts',(94.0461620117057,-0.897666917981372,
1.53274702655251));
#23068=CARTESIAN_POINT('Ctrl Pts',(94.0474203684577,-0.913842578200213,
1.52318245146987));
#23069=CARTESIAN_POINT('Ctrl Pts',(94.0481749850471,-0.923562911254201,
1.51730834175438));
#23070=CARTESIAN_POINT('Ctrl Pts',(94.0512503075312,-0.963222456067497,
1.49281927218814));
#23071=CARTESIAN_POINT('Ctrl Pts',(94.0535248315128,-0.992662692539539,
1.47340695244934));
#23072=CARTESIAN_POINT('Ctrl Pts',(94.0599345840296,-1.07517503531732,1.41540318285753));
#23073=CARTESIAN_POINT('Ctrl Pts',(94.0639826484755,-1.12671492843033,1.37472985710406));
#23074=CARTESIAN_POINT('Ctrl Pts',(94.0760163600187,-1.27347719665078,1.24509961434019));
#23075=CARTESIAN_POINT('Ctrl Pts',(94.0839474661905,-1.36128145355664,1.14844501713842));
#23076=CARTESIAN_POINT('Ctrl Pts',(94.0940232074457,-1.45303593928849,1.0219734796882));
#23077=CARTESIAN_POINT('Ctrl Pts',(94.0957195603368,-1.46787292796113,1.00054594499747));
#23078=CARTESIAN_POINT('Ctrl Pts',(94.0984007307722,-1.49033478617992,0.966531154926721));
#23079=CARTESIAN_POINT('Ctrl Pts',(94.0993733655579,-1.49828413252358,0.954161875537906));
#23080=CARTESIAN_POINT('Ctrl Pts',(94.1011890951546,-1.51275023442366,0.931025855163851));
#23081=CARTESIAN_POINT('Ctrl Pts',(94.1020306049174,-1.51930793288489,0.920285719623472));
#23082=CARTESIAN_POINT('Ctrl Pts',(94.1039127653671,-1.5336465055089,0.896231139049658));
#23083=CARTESIAN_POINT('Ctrl Pts',(94.1049554542481,-1.5413691387209,0.882883350427976));
#23084=CARTESIAN_POINT('Ctrl Pts',(94.1080759892758,-1.56382181252274,0.842883533271501));
#23085=CARTESIAN_POINT('Ctrl Pts',(94.1101716969438,-1.57804068406961,0.815952640954332));
#23086=CARTESIAN_POINT('Ctrl Pts',(94.1210439991829,-1.64740550188712,0.675972541353107));
#23087=CARTESIAN_POINT('Ctrl Pts',(94.1302005745206,-1.69111464581896,0.557678276784016));
#23088=CARTESIAN_POINT('Ctrl Pts',(94.1457148620955,-1.74316211221659,0.352017368228739));
#23089=CARTESIAN_POINT('Ctrl Pts',(94.1520214378522,-1.75822269099445,0.266807217441393));
#23090=CARTESIAN_POINT('Ctrl Pts',(94.1593606225872,-1.76887433059878,0.16272377323222));
#23091=CARTESIAN_POINT('Ctrl Pts',(94.1606260255372,-1.77044914422218,0.144586707148865));
#23092=CARTESIAN_POINT('Ctrl Pts',(94.1624864399562,-1.77237554125064,0.117590392395109));
#23093=CARTESIAN_POINT('Ctrl Pts',(94.163092114422,-1.77294004511353,0.108748170059994));
#23094=CARTESIAN_POINT('Ctrl Pts',(94.164176593029,-1.77383771797021,0.0928128560022862));
#23095=CARTESIAN_POINT('Ctrl Pts',(94.164656633065,-1.77419454460256,0.0857216320530697));
#23096=CARTESIAN_POINT('Ctrl Pts',(94.1657382355763,-1.77490624882382,0.0696596089174864));
#23097=CARTESIAN_POINT('Ctrl Pts',(94.1663383967329,-1.77523565268846,0.060688049386925));
#23098=CARTESIAN_POINT('Ctrl Pts',(94.1681861506817,-1.77604505875409,0.0328987805694946));
#23099=CARTESIAN_POINT('Ctrl Pts',(94.1694218314036,-1.77629399169738,0.014074975118532));
#23100=CARTESIAN_POINT('Ctrl Pts',(94.1723362417095,-1.77617402467342,-0.0307849275125319));
#23101=CARTESIAN_POINT('Ctrl Pts',(94.1740030436563,-1.77553200855828,-0.0568164163390386));
#23102=CARTESIAN_POINT('Ctrl Pts',(94.1804817763263,-1.77076266237805,-0.158986852576733));
#23103=CARTESIAN_POINT('Ctrl Pts',(94.1851563792875,-1.76230713983039,-0.234845329123573));
#23104=CARTESIAN_POINT('Ctrl Pts',(94.1968509995233,-1.72906222918476,-0.422453601548267));
#23105=CARTESIAN_POINT('Ctrl Pts',(94.2038652132316,-1.69831305992961,-0.532777844206003));
#23106=CARTESIAN_POINT('Ctrl Pts',(94.2128035603766,-1.64836806490588,-0.662228512982705));
#23107=CARTESIAN_POINT('Ctrl Pts',(94.2143951616313,-1.63908094679585,-0.684892281594365));
#23108=CARTESIAN_POINT('Ctrl Pts',(94.2170265869908,-1.62311268248434,-0.721673691903877));
#23109=CARTESIAN_POINT('Ctrl Pts',(94.2180570756095,-1.61670850102209,-0.735908482348476));
#23110=CARTESIAN_POINT('Ctrl Pts',(94.2199306990669,-1.60479962043342,-0.761472817450772));
#23111=CARTESIAN_POINT('Ctrl Pts',(94.2207715305944,-1.59936037611383,-0.772831835991971));
#23112=CARTESIAN_POINT('Ctrl Pts',(94.2225932872729,-1.58737539432715,-0.797192121874985));
#23113=CARTESIAN_POINT('Ctrl Pts',(94.2235755619921,-1.58078975178258,-0.810172611451816));
#23114=CARTESIAN_POINT('Ctrl Pts',(94.2263336906443,-1.56196047538652,-0.846181850452954));
#23115=CARTESIAN_POINT('Ctrl Pts',(94.2281216997987,-1.54936850242923,-0.869023226657982));
#23116=CARTESIAN_POINT('Ctrl Pts',(94.2359229917443,-1.49280695684608,-0.966484463187603));
#23117=CARTESIAN_POINT('Ctrl Pts',(94.2421084162089,-1.44392116365872,-1.03810050837571));
#23118=CARTESIAN_POINT('Ctrl Pts',(94.2581282650563,-1.30660611156105,-1.2106995315271));
#23119=CARTESIAN_POINT('Ctrl Pts',(94.2680783984377,-1.21160243492819,-1.30576991082433));
#23120=CARTESIAN_POINT('Ctrl Pts',(94.278692807597,-1.09312175316951,-1.4001625643195));
#23121=CARTESIAN_POINT('Ctrl Pts',(94.279908373913,-1.07927203307594,-1.41086580156895));
#23122=CARTESIAN_POINT('Ctrl Pts',(94.281710327571,-1.05828459896727,-1.42659520595447));
#23123=CARTESIAN_POINT('Ctrl Pts',(94.2823064649139,-1.05126482115094,-1.43177598037084));
#23124=CARTESIAN_POINT('Ctrl Pts',(94.2833332810544,-1.03903547822782,-1.44066311313724));
#23125=CARTESIAN_POINT('Ctrl Pts',(94.2837655490933,-1.0338437983784,-1.4443932755476));
#23126=CARTESIAN_POINT('Ctrl Pts',(94.2847846872879,-1.02150089251405,-1.45316086406434));
#23127=CARTESIAN_POINT('Ctrl Pts',(94.2853698915786,-1.01433246163006,-1.45817359584425));
#23128=CARTESIAN_POINT('Ctrl Pts',(94.2871237602798,-0.992614842103307,
-1.47312261195568));
#23129=CARTESIAN_POINT('Ctrl Pts',(94.2882821884218,-0.977954084614268,
-1.48289592375008));
#23130=CARTESIAN_POINT('Ctrl Pts',(94.2940509198816,-0.903503194083136,
-1.53094266156814));
#23131=CARTESIAN_POINT('Ctrl Pts',(94.2984845150199,-0.841595962509255,
-1.56582945647219));
#23132=CARTESIAN_POINT('Ctrl Pts',(94.3108614411569,-0.661391893625565,
-1.65359566043891));
#23133=CARTESIAN_POINT('Ctrl Pts',(94.3186796817457,-0.53918478404979,-1.69737919369666));
#23134=CARTESIAN_POINT('Ctrl Pts',(94.3293390681498,-0.376219298444444,
-1.73636900249191));
#23135=CARTESIAN_POINT('Ctrl Pts',(94.3317952242991,-0.338858081628253,
-1.74404505191454));
#23136=CARTESIAN_POINT('Ctrl Pts',(94.3353011701874,-0.286028070785535,
-1.75313762786081));
#23137=CARTESIAN_POINT('Ctrl Pts',(94.3363193742529,-0.270742100845669,
-1.75556323991451));
#23138=CARTESIAN_POINT('Ctrl Pts',(94.3381942993764,-0.242713527250378,
-1.75963611172289));
#23139=CARTESIAN_POINT('Ctrl Pts',(94.3390490058336,-0.229980905755203,
-1.76134547155717));
#23140=CARTESIAN_POINT('Ctrl Pts',(94.3407973754078,-0.204033453615995,
-1.76454278383942));
#23141=CARTESIAN_POINT('Ctrl Pts',(94.3416912957212,-0.190818241230066,
-1.76602074401358));
#23142=CARTESIAN_POINT('Ctrl Pts',(94.3439433435283,-0.157662034001186,
-1.76935236682008));
#23143=CARTESIAN_POINT('Ctrl Pts',(94.3453072936736,-0.137704393111346,
-1.77101737927376));
#23144=CARTESIAN_POINT('Ctrl Pts',(94.3510767812486,-0.053830993602963,
-1.77658846035042));
#23145=CARTESIAN_POINT('Ctrl Pts',(94.355577273278,0.0102367710365958,-1.77737385486933));
#23146=CARTESIAN_POINT('Ctrl Pts',(94.3703551594012,0.216494383810738,-1.76875015293116));
#23147=CARTESIAN_POINT('Ctrl Pts',(94.3809506457999,0.357540539793017,-1.7457109125371));
#23148=CARTESIAN_POINT('Ctrl Pts',(94.3937151254229,0.52878488348619,-1.69609507560905));
#23149=CARTESIAN_POINT('Ctrl Pts',(94.3962529888944,0.562946730654938,-1.68506478965365));
#23150=CARTESIAN_POINT('Ctrl Pts',(94.3995567543169,0.60784249456448,-1.66905068142524));
#23151=CARTESIAN_POINT('Ctrl Pts',(94.4003672915372,0.618892347483565,-1.66498497183998));
#23152=CARTESIAN_POINT('Ctrl Pts',(94.4016346862455,0.636238535227415,-1.65840601964273));
#23153=CARTESIAN_POINT('Ctrl Pts',(94.4020956588359,0.642562070255365,-1.65596618005126));
#23154=CARTESIAN_POINT('Ctrl Pts',(94.4030536815524,0.655737487206398,-1.65079581111914));
#23155=CARTESIAN_POINT('Ctrl Pts',(94.4035502873442,0.662586578068556,-1.64805870387988));
#23156=CARTESIAN_POINT('Ctrl Pts',(94.4047855405379,0.679665399435131,-1.64110980368981));
#23157=CARTESIAN_POINT('Ctrl Pts',(94.4055210822748,0.689873430413712,-1.63684486392991));
#23158=CARTESIAN_POINT('Ctrl Pts',(94.408409929064,0.730082635461765,-1.61960237270646));
#23159=CARTESIAN_POINT('Ctrl Pts',(94.4105238008715,0.75976494654413,-1.60589228894177));
#23160=CARTESIAN_POINT('Ctrl Pts',(94.4162986603034,0.840944945395216,-1.5656405459852));
#23161=CARTESIAN_POINT('Ctrl Pts',(94.4198917248216,0.891550042316297,-1.53738679760621));
#23162=CARTESIAN_POINT('Ctrl Pts',(94.4323339885751,1.06288894054865,-1.4304143849655));
#23163=CARTESIAN_POINT('Ctrl Pts',(94.441054845466,1.17534282806859,-1.33954600846397));
#23164=CARTESIAN_POINT('Ctrl Pts',(94.4519422362075,1.29258283149604,-1.2185606803535));
#23165=CARTESIAN_POINT('Ctrl Pts',(94.4535345871111,1.30921412411718,-1.20067430681051));
#23166=CARTESIAN_POINT('Ctrl Pts',(94.4560872195412,1.33502222955283,-1.17174467117599));
#23167=CARTESIAN_POINT('Ctrl Pts',(94.4570372016982,1.34444338902761,-1.16092285754837));
#23168=CARTESIAN_POINT('Ctrl Pts',(94.4587487780797,1.36108341582007,-1.14133471159695));
#23169=CARTESIAN_POINT('Ctrl Pts',(94.4595082920185,1.36835134784434,-1.13261095140028));
#23170=CARTESIAN_POINT('Ctrl Pts',(94.4612985729268,1.3852080404834,-1.11197863827282));
#23171=CARTESIAN_POINT('Ctrl Pts',(94.4623320581621,1.39472754428421,-1.10001493584488));
#23172=CARTESIAN_POINT('Ctrl Pts',(94.4653958477792,1.42232068283326,-1.06440301540969));
#23173=CARTESIAN_POINT('Ctrl Pts',(94.4674430511485,1.4399549523948,-1.04042272801189));
#23174=CARTESIAN_POINT('Ctrl Pts',(94.474467851913,1.49773733161957,-0.957561861929908));
#23175=CARTESIAN_POINT('Ctrl Pts',(94.4795479971308,1.53493812033648,-0.896718831366329));
#23176=CARTESIAN_POINT('Ctrl Pts',(94.4923147950042,1.61771367677764,-0.74102002535935));
#23177=CARTESIAN_POINT('Ctrl Pts',(94.5000769950445,1.65871199671132,-0.644035723222692));
#23178=CARTESIAN_POINT('Ctrl Pts',(94.5109847202854,1.70502685167466,-0.500076256215709));
#23179=CARTESIAN_POINT('Ctrl Pts',(94.514270935289,1.71744200492499,-0.455616691109116));
#23180=CARTESIAN_POINT('Ctrl Pts',(94.5183643008631,1.73106738122804,-0.398287690991768));
#23181=CARTESIAN_POINT('Ctrl Pts',(94.5192456907559,1.73388809172322,-0.385823110128413));
#23182=CARTESIAN_POINT('Ctrl Pts',(94.5206493463459,1.73820094271484,-0.365761472941479));
#23183=CARTESIAN_POINT('Ctrl Pts',(94.5211761528115,1.7397783109951,-0.358183481934652));
#23184=CARTESIAN_POINT('Ctrl Pts',(94.5221990240581,1.74276093592466,-0.343369638293446));
#23185=CARTESIAN_POINT('Ctrl Pts',(94.522695311691,1.74417076744543,-0.336134980253873));
#23186=CARTESIAN_POINT('Ctrl Pts',(94.5236944786626,1.74693220727491,-0.32147911596434));
#23187=CARTESIAN_POINT('Ctrl Pts',(94.524197237557,1.74828166772825,-0.314057596849312));
#23188=CARTESIAN_POINT('Ctrl Pts',(94.525411204536,1.75144109941514,-0.296030218846623));
#23189=CARTESIAN_POINT('Ctrl Pts',(94.5261198851904,1.75320209134581,-0.28541593402213));
#23190=CARTESIAN_POINT('Ctrl Pts',(94.5318074522998,1.76664475776472,-0.199566997261982));
#23191=CARTESIAN_POINT('Ctrl Pts',(94.5365633824408,1.77357534152074,-0.123668924889746));
#23192=CARTESIAN_POINT('Ctrl Pts',(94.5412649413994,1.77561364082573,-0.0475422024479729));
#23193=CARTESIAN_POINT('Origin',(88.3562164250559,0.,0.));
#23194=CARTESIAN_POINT('',(95.4381488386039,1.77561363782275,-0.0475423146035081));
#23195=CARTESIAN_POINT('',(95.2889037169481,1.77561363837214,-0.0475422940850334));
#23196=CARTESIAN_POINT('',(88.3562164250559,1.77561363837197,-0.0475422940912398));
#23197=CARTESIAN_POINT('Ctrl Pts',(95.4381488398588,1.77561363782069,-0.0475423146804766));
#23198=CARTESIAN_POINT('Ctrl Pts',(95.4371673493555,1.77518568041986,-0.0635256971142646));
#23199=CARTESIAN_POINT('Ctrl Pts',(95.4361859452281,1.77454179510398,-0.0795075586954785));
#23200=CARTESIAN_POINT('Ctrl Pts',(95.4286895757639,1.76798043142665,-0.201390030257114));
#23201=CARTESIAN_POINT('Ctrl Pts',(95.4221357747288,1.75280626594391,-0.306560285918419));
#23202=CARTESIAN_POINT('Ctrl Pts',(95.4136906852217,1.72266583260142,-0.43369635086399));
#23203=CARTESIAN_POINT('Ctrl Pts',(95.412085225413,1.71648992989322,-0.457528490473432));
#23204=CARTESIAN_POINT('Ctrl Pts',(95.4095192272436,1.70593506054631,-0.49503067106221));
#23205=CARTESIAN_POINT('Ctrl Pts',(95.4085692527349,1.70188212861389,-0.508789736578343));
#23206=CARTESIAN_POINT('Ctrl Pts',(95.4067632719889,1.69390719590134,-0.534701323316748));
#23207=CARTESIAN_POINT('Ctrl Pts',(95.4059084524313,1.6900198952807,-0.546863632288354));
#23208=CARTESIAN_POINT('Ctrl Pts',(95.4039514683984,1.68086779615735,-0.574468165148865));
#23209=CARTESIAN_POINT('Ctrl Pts',(95.402846645943,1.67552075057792,-0.589881686674298));
#23210=CARTESIAN_POINT('Ctrl Pts',(95.3999171180912,1.6608754492379,-0.63029202402014));
#23211=CARTESIAN_POINT('Ctrl Pts',(95.3980809603956,1.65122552306115,-0.655156036148417));
#23212=CARTESIAN_POINT('Ctrl Pts',(95.3865169487597,1.5875710967022,-0.808817955858918));
#23213=CARTESIAN_POINT('Ctrl Pts',(95.3762999014666,1.51909945304612,-0.931070379372612));
#23214=CARTESIAN_POINT('Ctrl Pts',(95.3606835981856,1.39343576093228,-1.10404017970042));
#23215=CARTESIAN_POINT('Ctrl Pts',(95.3552972034587,1.34610869587555,-1.16127576580758));
#23216=CARTESIAN_POINT('Ctrl Pts',(95.3488288491492,1.28299642352949,-1.22853957113195));
#23217=CARTESIAN_POINT('Ctrl Pts',(95.347575452205,1.27045634253153,-1.24150313935822));
#23218=CARTESIAN_POINT('Ctrl Pts',(95.3457255077907,1.25145014069643,-1.26056156399679));
#23219=CARTESIAN_POINT('Ctrl Pts',(95.3451185600749,1.24513264638749,-1.2668021205742));
#23220=CARTESIAN_POINT('Ctrl Pts',(95.3440763856211,1.23413857505972,-1.27750059661218));
#23221=CARTESIAN_POINT('Ctrl Pts',(95.3436394845621,1.2294842032969,-1.28198065284727));
#23222=CARTESIAN_POINT('Ctrl Pts',(95.3426132321228,1.21844398021522,-1.29249196382069));
#23223=CARTESIAN_POINT('Ctrl Pts',(95.3420255357341,1.21203771329877,-1.2985013666496));
#23224=CARTESIAN_POINT('Ctrl Pts',(95.3403105965251,1.19310624920436,-1.31599785640673));
#23225=CARTESIAN_POINT('Ctrl Pts',(95.33919262212,1.18046007286718,-1.32735336225359));
#23226=CARTESIAN_POINT('Ctrl Pts',(95.3308679771558,1.08417677787222,-1.4113453066066));
#23227=CARTESIAN_POINT('Ctrl Pts',(95.3241108295041,0.994060706740887,-1.47620620847798));
#23228=CARTESIAN_POINT('Ctrl Pts',(95.3152906131993,0.870110629089963,-1.54888764775307));
#23229=CARTESIAN_POINT('Ctrl Pts',(95.3132708506961,0.841287212199349,-1.56473040189169));
#23230=CARTESIAN_POINT('Ctrl Pts',(95.3077199227652,0.761360968934005,-1.60581463858947));
#23231=CARTESIAN_POINT('Ctrl Pts',(95.3041682495723,0.709459670634261,-1.6294101537994));
#23232=CARTESIAN_POINT('Ctrl Pts',(95.2980575322972,0.620178695072255,-1.66492398051627));
#23233=CARTESIAN_POINT('Ctrl Pts',(95.2955386072899,0.583375197136572,-1.67817355998439));
#23234=CARTESIAN_POINT('Ctrl Pts',(95.2918653442918,0.529955168111838,-1.6954355871143));
#23235=CARTESIAN_POINT('Ctrl Pts',(95.2907433566947,0.513669833561855,-1.70044040733465));
#23236=CARTESIAN_POINT('Ctrl Pts',(95.2887611114122,0.484971922091875,-1.70881000125862));
#23237=CARTESIAN_POINT('Ctrl Pts',(95.2879042108289,0.472589920062627,-1.71227571908705));
#23238=CARTESIAN_POINT('Ctrl Pts',(95.2861066928904,0.446673244280947,-1.7192272658083));
#23239=CARTESIAN_POINT('Ctrl Pts',(95.2851653403585,0.43313291846677,-1.72268837406661));
#23240=CARTESIAN_POINT('Ctrl Pts',(95.2826705018581,0.397341387506327,-1.7313885798578));
#23241=CARTESIAN_POINT('Ctrl Pts',(95.2811085177059,0.375028081133695,-1.73635838637605));
#23242=CARTESIAN_POINT('Ctrl Pts',(95.272573753399,0.253673389488195,-1.76093930008252));
#23243=CARTESIAN_POINT('Ctrl Pts',(95.2653503297794,0.153208476465598,-1.77250627066225));
#23244=CARTESIAN_POINT('Ctrl Pts',(95.2524947111216,-0.0232766188042014,
-1.777706985077));
#23245=CARTESIAN_POINT('Ctrl Pts',(95.2469347538782,-0.0989381650435437,
-1.77510427009905));
#23246=CARTESIAN_POINT('Ctrl Pts',(95.2372981268782,-0.231157724342564,
-1.76207419550361));
#23247=CARTESIAN_POINT('Ctrl Pts',(95.2331963121733,-0.287813675324886,
-1.75371149143344));
#23248=CARTESIAN_POINT('Ctrl Pts',(95.2282984974795,-0.356926834026268,
-1.74006944161283));
#23249=CARTESIAN_POINT('Ctrl Pts',(95.2273871231394,-0.369853145243995,
-1.73736786649673));
#23250=CARTESIAN_POINT('Ctrl Pts',(95.2259440168215,-0.390445251720871,
-1.73282390647435));
#23251=CARTESIAN_POINT('Ctrl Pts',(95.2254073726865,-0.398130703375255,
-1.73107427182585));
#23252=CARTESIAN_POINT('Ctrl Pts',(95.2243777491388,-0.412935198287473,
-1.72760013670458));
#23253=CARTESIAN_POINT('Ctrl Pts',(95.2238844162702,-0.420055584077246,
-1.72588267819068));
#23254=CARTESIAN_POINT('Ctrl Pts',(95.2226628087831,-0.437748554545267,
-1.72149909884819));
#23255=CARTESIAN_POINT('Ctrl Pts',(95.2219375190404,-0.448307829774046,
-1.71877952312162));
#23256=CARTESIAN_POINT('Ctrl Pts',(95.2193284152843,-0.486459698973201,
-1.70857786291976));
#23257=CARTESIAN_POINT('Ctrl Pts',(95.2174738067635,-0.513897230877726,
-1.70052674397468));
#23258=CARTESIAN_POINT('Ctrl Pts',(95.2087784569228,-0.643299296123917,
-1.65913727985531));
#23259=CARTESIAN_POINT('Ctrl Pts',(95.2022685206178,-0.742307887420377,
-1.61726742379149));
#23260=CARTESIAN_POINT('Ctrl Pts',(95.1914301637065,-0.897823080502049,
-1.53419108528537));
#23261=CARTESIAN_POINT('Ctrl Pts',(95.1871635416619,-0.956755050066244,
-1.49814797876201));
#23262=CARTESIAN_POINT('Ctrl Pts',(95.1808766824735,-1.03832904654075,-1.44147684478382));
#23263=CARTESIAN_POINT('Ctrl Pts',(95.1789401966896,-1.06277296510262,-1.42355055125931));
#23264=CARTESIAN_POINT('Ctrl Pts',(95.1753900523547,-1.10622005712269,-1.38994511258567));
#23265=CARTESIAN_POINT('Ctrl Pts',(95.1737844180664,-1.12537867034144,-1.37447916773796));
#23266=CARTESIAN_POINT('Ctrl Pts',(95.1712182059507,-1.15518037168218,-1.34938064361897));
#23267=CARTESIAN_POINT('Ctrl Pts',(95.1702681950715,-1.16603921285925,-1.34000833811395));
#23268=CARTESIAN_POINT('Ctrl Pts',(95.1684621854115,-1.18634719608626,-1.32204667891708));
#23269=CARTESIAN_POINT('Ctrl Pts',(95.1676073738127,-1.19581958962775,-1.31348490103295));
#23270=CARTESIAN_POINT('Ctrl Pts',(95.1656504647123,-1.21718236025994,-1.29375318013663));
#23271=CARTESIAN_POINT('Ctrl Pts',(95.1645457099933,-1.2290126558104,-1.28252019479913));
#23272=CARTESIAN_POINT('Ctrl Pts',(95.1610614953316,-1.26559593827056,-1.24681298083359));
#23273=CARTESIAN_POINT('Ctrl Pts',(95.15865759349,-1.28978395456291,-1.2217744241541));
#23274=CARTESIAN_POINT('Ctrl Pts',(95.1468741443294,-1.40325543831654,-1.09718612430613));
#23275=CARTESIAN_POINT('Ctrl Pts',(95.1370764576979,-1.48182889672163,-0.988491527100039));
#23276=CARTESIAN_POINT('Ctrl Pts',(95.1220377431135,-1.58294661753013,-0.809055304563493));
#23277=CARTESIAN_POINT('Ctrl Pts',(95.1167940145574,-1.61456416910075,-0.74395901525983));
#23278=CARTESIAN_POINT('Ctrl Pts',(95.1104747571104,-1.64892543675146,-0.660626160949176));
#23279=CARTESIAN_POINT('Ctrl Pts',(95.1092357826179,-1.65547451529085,-0.64403898209159));
#23280=CARTESIAN_POINT('Ctrl Pts',(95.1074027617619,-1.66489532664284,-0.619084619121653));
#23281=CARTESIAN_POINT('Ctrl Pts',(95.1067985800756,-1.66795595490535,-0.610790598500431));
#23282=CARTESIAN_POINT('Ctrl Pts',(95.1057592938277,-1.67314528261916,-0.596398055070963));
#23283=CARTESIAN_POINT('Ctrl Pts',(95.1053225464353,-1.67530277300227,-0.590310426058524));
#23284=CARTESIAN_POINT('Ctrl Pts',(95.10429396303,-1.68032840724935,-0.575880472599933));
#23285=CARTESIAN_POINT('Ctrl Pts',(95.1037038138373,-1.68316767180902,-0.567528388533941));
#23286=CARTESIAN_POINT('Ctrl Pts',(95.1019375237214,-1.6915268381239,-0.542324134058072));
#23287=CARTESIAN_POINT('Ctrl Pts',(95.1007717341914,-1.69685690947472,-0.525409552605657));
#23288=CARTESIAN_POINT('Ctrl Pts',(95.0929682560156,-1.73117212989926,-0.410538918989828));
#23289=CARTESIAN_POINT('Ctrl Pts',(95.0867074481429,-1.75191715264279,-0.31030759736876));
#23290=CARTESIAN_POINT('Ctrl Pts',(95.0778737458339,-1.76883750564417,-0.167391252180866));
#23291=CARTESIAN_POINT('Ctrl Pts',(95.0753140629568,-1.7722821364723,-0.125785145551214));
#23292=CARTESIAN_POINT('Ctrl Pts',(95.0685917547937,-1.77743291750523,-0.0171151289799343));
#23293=CARTESIAN_POINT('Ctrl Pts',(95.0644026470968,-1.77681196856192,0.0499871792206389));
#23294=CARTESIAN_POINT('Ctrl Pts',(95.0580791121454,-1.77031852771257,0.148447213957664));
#23295=CARTESIAN_POINT('Ctrl Pts',(95.0560300720526,-1.76739498630451,0.17994174175725));
#23296=CARTESIAN_POINT('Ctrl Pts',(95.0529224883144,-1.76176019168303,0.226964113105994));
#23297=CARTESIAN_POINT('Ctrl Pts',(95.0518836669746,-1.75968042886069,0.242562246299189));
#23298=CARTESIAN_POINT('Ctrl Pts',(95.0499932489024,-1.75554525894066,0.270715168917963));
#23299=CARTESIAN_POINT('Ctrl Pts',(95.0491439784046,-1.75356167329921,0.283279548020821));
#23300=CARTESIAN_POINT('Ctrl Pts',(95.0473018064264,-1.7489899892575,0.310346722133862));
#23301=CARTESIAN_POINT('Ctrl Pts',(95.0463075053272,-1.74635608218016,0.324840702310841));
#23302=CARTESIAN_POINT('Ctrl Pts',(95.0435574125313,-1.73861836309575,0.364602109211037));
#23303=CARTESIAN_POINT('Ctrl Pts',(95.0417900166289,-1.73314449965041,0.389792935171712));
#23304=CARTESIAN_POINT('Ctrl Pts',(95.0291919330397,-1.69064359333954,0.566732903912166));
#23305=CARTESIAN_POINT('Ctrl Pts',(95.0177192469712,-1.63429307894147,0.713112327410821));
#23306=CARTESIAN_POINT('Ctrl Pts',(95.0011850257931,-1.52570813381402,0.912293765463015));
#23307=CARTESIAN_POINT('Ctrl Pts',(94.9960788583705,-1.48817670967008,0.97231552266737));
#23308=CARTESIAN_POINT('Ctrl Pts',(94.9901925835517,-1.43914672742977,1.04120691544465));
#23309=CARTESIAN_POINT('Ctrl Pts',(94.9892375413963,-1.43099993238571,1.05237558269419));
#23310=CARTESIAN_POINT('Ctrl Pts',(94.9877419284562,-1.41792433995297,1.06986862620894));
#23311=CARTESIAN_POINT('Ctrl Pts',(94.9871958371664,-1.41308188664874,1.07625642818078));
#23312=CARTESIAN_POINT('Ctrl Pts',(94.9861609294346,-1.40377116982851,1.08836725256927));
#23313=CARTESIAN_POINT('Ctrl Pts',(94.9856716259847,-1.39931084979218,1.09409593783311));
#23314=CARTESIAN_POINT('Ctrl Pts',(94.9844779740392,-1.38828992691172,1.10807319971657));
#23315=CARTESIAN_POINT('Ctrl Pts',(94.9837763029032,-1.38169066719397,1.11629120345719));
#23316=CARTESIAN_POINT('Ctrl Pts',(94.9817446898492,-1.36224398336196,1.14007131244078));
#23317=CARTESIAN_POINT('Ctrl Pts',(94.9804272147335,-1.34920360346218,1.15547435513978));
#23318=CARTESIAN_POINT('Ctrl Pts',(94.9707807858997,-1.25079024058236,1.267779834886));
#23319=CARTESIAN_POINT('Ctrl Pts',(94.9630093783366,-1.15532892641939,1.35534688537089));
#23320=CARTESIAN_POINT('Ctrl Pts',(94.951279670803,-1.00194349411806,1.46796047754011));
#23321=CARTESIAN_POINT('Ctrl Pts',(94.9474820629408,-0.950851815255546,
1.50155877336549));
#23322=CARTESIAN_POINT('Ctrl Pts',(94.9418155820051,-0.873845596467484,
1.54669015914483));
#23323=CARTESIAN_POINT('Ctrl Pts',(94.9400121966892,-0.849223956355684,
1.56034455138024));
#23324=CARTESIAN_POINT('Ctrl Pts',(94.9366830482413,-0.803683841019369,
1.58420246710241));
#23325=CARTESIAN_POINT('Ctrl Pts',(94.9351638030877,-0.782869245339488,
1.59459111866113));
#23326=CARTESIAN_POINT('Ctrl Pts',(94.9327035142906,-0.749156372829304,
1.61059817305142));
#23327=CARTESIAN_POINT('Ctrl Pts',(94.9317715514774,-0.736384502070001,
1.6164775259447));
#23328=CARTESIAN_POINT('Ctrl Pts',(94.9299789232367,-0.711824923907548,
1.62743172273709));
#23329=CARTESIAN_POINT('Ctrl Pts',(94.9291191881015,-0.700049335813447,
1.63253166797313));
#23330=CARTESIAN_POINT('Ctrl Pts',(94.9271394605597,-0.672947568246527,
1.64392216153924));
#23331=CARTESIAN_POINT('Ctrl Pts',(94.9260166366948,-0.657586773182371,
1.65012669393636));
#23332=CARTESIAN_POINT('Ctrl Pts',(94.9223396594687,-0.607333137269243,
1.66961203095749));
#23333=CARTESIAN_POINT('Ctrl Pts',(94.9197565978034,-0.572109983229449,
1.68200703867904));
#23334=CARTESIAN_POINT('Ctrl Pts',(94.9079552575104,-0.411628399259981,
1.73285639979874));
#23335=CARTESIAN_POINT('Ctrl Pts',(94.8983488517735,-0.282752252931157,
1.75848530785277));
#23336=CARTESIAN_POINT('Ctrl Pts',(94.8849250549699,-0.0995456483039938,
1.77424735036882));
#23337=CARTESIAN_POINT('Ctrl Pts',(94.8810826290418,-0.0466558431728965,
1.77642531440982));
#23338=CARTESIAN_POINT('Ctrl Pts',(94.8758082839818,0.0273778155928267,
1.77616460167959));
#23339=CARTESIAN_POINT('Ctrl Pts',(94.874315572671,0.0484985309680788,1.77571343770735));
#23340=CARTESIAN_POINT('Ctrl Pts',(94.8717122731435,0.0857089449389605,
1.77425412688575));
#23341=CARTESIAN_POINT('Ctrl Pts',(94.8705951424533,0.101802150352386,1.77340353499224));
#23342=CARTESIAN_POINT('Ctrl Pts',(94.8689059522415,0.126361207220014,1.77177005243482));
#23343=CARTESIAN_POINT('Ctrl Pts',(94.868325878031,0.134836238578159,1.77114524240381));
#23344=CARTESIAN_POINT('Ctrl Pts',(94.867259981052,0.150491967884848,1.76987801747836));
#23345=CARTESIAN_POINT('Ctrl Pts',(94.8667732932794,0.157673428877371,1.76925270146217));
#23346=CARTESIAN_POINT('Ctrl Pts',(94.865651562348,0.174299328095295,1.76770298628976));
#23347=CARTESIAN_POINT('Ctrl Pts',(94.865018285955,0.183740424727292,1.76674660604242));
#23348=CARTESIAN_POINT('Ctrl Pts',(94.8629324881069,0.21499912065253,1.76332682518299));
#23349=CARTESIAN_POINT('Ctrl Pts',(94.8614968053256,0.236779639654297,1.76053447082646));
#23350=CARTESIAN_POINT('Ctrl Pts',(94.8527390632201,0.370827037566415,1.7408161429651));
#23351=CARTESIAN_POINT('Ctrl Pts',(94.8458471554891,0.481320864256407,1.71356059277393));
#23352=CARTESIAN_POINT('Ctrl Pts',(94.833366047352,0.672993875978803,1.64625910565092));
#23353=CARTESIAN_POINT('Ctrl Pts',(94.8278284177559,0.755146664504372,1.61023013540792));
#23354=CARTESIAN_POINT('Ctrl Pts',(94.8200076135586,0.863001729550939,1.55285362419956));
#23355=CARTESIAN_POINT('Ctrl Pts',(94.8178976331551,0.89134805181674,1.53675788581653));
#23356=CARTESIAN_POINT('Ctrl Pts',(94.8147161836586,0.932852470792316,1.51165592143452));
#23357=CARTESIAN_POINT('Ctrl Pts',(94.813665901402,0.946359035998366,1.50323714183039));
#23358=CARTESIAN_POINT('Ctrl Pts',(94.8117710409134,0.97036583562552,1.48782168372529));
#23359=CARTESIAN_POINT('Ctrl Pts',(94.8109290072689,0.980908212262696,1.48089239396712));
#23360=CARTESIAN_POINT('Ctrl Pts',(94.8091061685265,1.00345469925942,1.46572666145408));
#23361=CARTESIAN_POINT('Ctrl Pts',(94.8081240270271,1.01543308136226,1.45745381224456));
#23362=CARTESIAN_POINT('Ctrl Pts',(94.8054415087653,1.04768237545668,1.43459034479831));
#23363=CARTESIAN_POINT('Ctrl Pts',(94.8037304481028,1.06774875663906,1.41971838730255));
#23364=CARTESIAN_POINT('Ctrl Pts',(94.7922848369348,1.19860504596151,1.31839219500686));
#23365=CARTESIAN_POINT('Ctrl Pts',(94.7820407735927,1.29909441720299,1.21948811449991));
#23366=CARTESIAN_POINT('Ctrl Pts',(94.7674146906,1.42410518327764,1.06326908561091));
#23367=CARTESIAN_POINT('Ctrl Pts',(94.7630708283233,1.45898217969909,1.0148834998749));
#23368=CARTESIAN_POINT('Ctrl Pts',(94.7564345086485,1.5094665079192,0.936848885948652));
#23369=CARTESIAN_POINT('Ctrl Pts',(94.7540834939636,1.52678122949233,0.908358073211197));
#23370=CARTESIAN_POINT('Ctrl Pts',(94.7510008735257,1.54883263863395,0.869659173160387));
#23371=CARTESIAN_POINT('Ctrl Pts',(94.7502304010801,1.55428812154426,0.85987096217953));
#23372=CARTESIAN_POINT('Ctrl Pts',(94.748956687236,1.56321869611005,0.843485006820129));
#23373=CARTESIAN_POINT('Ctrl Pts',(94.7484503191297,1.5667454694961,0.83691593964364));
#23374=CARTESIAN_POINT('Ctrl Pts',(94.747484178333,1.57343084231696,0.824273198811469));
#23375=CARTESIAN_POINT('Ctrl Pts',(94.7470239780714,1.57659584239097,0.818203199452427));
#23376=CARTESIAN_POINT('Ctrl Pts',(94.7457701592087,1.58516256159992,0.801539219495063));
#23377=CARTESIAN_POINT('Ctrl Pts',(94.7449808330366,1.59049323025127,0.790908825815355));
#23378=CARTESIAN_POINT('Ctrl Pts',(94.7418039713718,1.61167083750602,0.747596382175172));
#23379=CARTESIAN_POINT('Ctrl Pts',(94.7394648128184,1.62662150386868,0.714483127974592));
#23380=CARTESIAN_POINT('Ctrl Pts',(94.7299363124912,1.68420417403958,0.57575111017351));
#23381=CARTESIAN_POINT('Ctrl Pts',(94.7230628628197,1.71764776153717,0.466608138897889));
#23382=CARTESIAN_POINT('Ctrl Pts',(94.7116571116216,1.75458779890793,0.285510854090841));
#23383=CARTESIAN_POINT('Ctrl Pts',(94.7072338745856,1.76458718397845,0.215233541031594));
#23384=CARTESIAN_POINT('Ctrl Pts',(94.7006555627475,1.77294188471233,0.112910995989636));
#23385=CARTESIAN_POINT('Ctrl Pts',(94.6985990062708,1.77467650086268,0.0812092230829106));
#23386=CARTESIAN_POINT('Ctrl Pts',(94.6954823038842,1.77599967523665,0.0337273940316071));
#23387=CARTESIAN_POINT('Ctrl Pts',(94.6944420581689,1.77622898703791,0.0179705997162901));
#23388=CARTESIAN_POINT('Ctrl Pts',(94.692550137101,1.77626447216838,-0.0105080252660238));
#23389=CARTESIAN_POINT('Ctrl Pts',(94.6917008055914,1.77614366013113,-0.0232288134528812));
#23390=CARTESIAN_POINT('Ctrl Pts',(94.6905877131099,1.77580798056828,-0.0398123924314369));
#23391=CARTESIAN_POINT('Ctrl Pts',(94.6903278697093,1.77571711781477,-0.0436775350756413));
#23392=CARTESIAN_POINT('Ctrl Pts',(94.6900676319114,1.77561363837047,-0.0475422941472846));
#23393=CARTESIAN_POINT('Ctrl Pts',(94.5412649413993,1.77561364082569,-0.0475422024493503));
#23394=CARTESIAN_POINT('Ctrl Pts',(94.5502559495098,1.77951157462697,0.098038441105544));
#23395=CARTESIAN_POINT('Ctrl Pts',(94.5590380957431,1.76549338159589,0.243522831115066));
#23396=CARTESIAN_POINT('Ctrl Pts',(94.5696946412978,1.72953923387427,0.405162651961136));
#23397=CARTESIAN_POINT('Ctrl Pts',(94.5709887792827,1.72487570912236,0.424577995570075));
#23398=CARTESIAN_POINT('Ctrl Pts',(94.5734554249558,1.71543901027195,0.461139564574982));
#23399=CARTESIAN_POINT('Ctrl Pts',(94.5746257052108,1.71073347462111,0.478300780756946));
#23400=CARTESIAN_POINT('Ctrl Pts',(94.5766571541859,1.70218030655673,0.507751936600956));
#23401=CARTESIAN_POINT('Ctrl Pts',(94.5775142851384,1.69845532226753,0.520076271800486));
#23402=CARTESIAN_POINT('Ctrl Pts',(94.5791707182688,1.69103671048592,0.543691090814504));
#23403=CARTESIAN_POINT('Ctrl Pts',(94.5799693212022,1.68736314076384,0.554987186979495));
#23404=CARTESIAN_POINT('Ctrl Pts',(94.5820904277551,1.6773531555736,0.584749156719975));
#23405=CARTESIAN_POINT('Ctrl Pts',(94.5834191879829,1.67082527805208,0.603148424399207));
#23406=CARTESIAN_POINT('Ctrl Pts',(94.5884755603374,1.6450303496808,0.672218558225581));
#23407=CARTESIAN_POINT('Ctrl Pts',(94.5922687211216,1.62375216049124,0.722101444863878));
#23408=CARTESIAN_POINT('Ctrl Pts',(94.6043363441921,1.55014513178004,0.874888580446807));
#23409=CARTESIAN_POINT('Ctrl Pts',(94.6128273086695,1.49005336935094,0.973712499303621));
#23410=CARTESIAN_POINT('Ctrl Pts',(94.624698448276,1.39228204238029,1.10402667664025));
#23411=CARTESIAN_POINT('Ctrl Pts',(94.6281401868569,1.36223387969837,1.14089596374243));
#23412=CARTESIAN_POINT('Ctrl Pts',(94.6335497010757,1.31182967650287,1.19790739923428));
#23413=CARTESIAN_POINT('Ctrl Pts',(94.6355561502634,1.29240414132561,1.21884002025618));
#23414=CARTESIAN_POINT('Ctrl Pts',(94.6382151437266,1.26556468839836,1.24639815128867));
#23415=CARTESIAN_POINT('Ctrl Pts',(94.6388963698949,1.25858874815304,1.25344194380564));
#23416=CARTESIAN_POINT('Ctrl Pts',(94.640080319447,1.24628315255528,1.26566091039485));
#23417=CARTESIAN_POINT('Ctrl Pts',(94.6405849629846,1.24097936442515,1.27086169995238));
#23418=CARTESIAN_POINT('Ctrl Pts',(94.6416045169882,1.23014106483343,1.28135696762661));
#23419=CARTESIAN_POINT('Ctrl Pts',(94.6421192643879,1.22460466216027,1.28664919262809));
#23420=CARTESIAN_POINT('Ctrl Pts',(94.6434607628024,1.2100124586053,1.30041830527501));
#23421=CARTESIAN_POINT('Ctrl Pts',(94.6442832082423,1.20090160889034,1.30883660782394));
#23422=CARTESIAN_POINT('Ctrl Pts',(94.647875443551,1.16042134111926,1.34546123258851));
#23423=CARTESIAN_POINT('Ctrl Pts',(94.6505790629205,1.12813855705992,1.37264257454532));
#23424=CARTESIAN_POINT('Ctrl Pts',(94.6593501812457,1.01864791992076,1.45835591298329));
#23425=CARTESIAN_POINT('Ctrl Pts',(94.665229264986,0.937620006526667,1.51172635659943));
#23426=CARTESIAN_POINT('Ctrl Pts',(94.676708788289,0.774000347592944,1.60125681749302));
#23427=CARTESIAN_POINT('Ctrl Pts',(94.6822812130052,0.692224483696,1.63826816696401));
#23428=CARTESIAN_POINT('Ctrl Pts',(94.6897675460822,0.583128412913388,1.67801269352639));
#23429=CARTESIAN_POINT('Ctrl Pts',(94.6914913025692,0.558047931298493,1.68651941377115));
#23430=CARTESIAN_POINT('Ctrl Pts',(94.6941963081379,0.518824328153877,1.6988524452324));
#23431=CARTESIAN_POINT('Ctrl Pts',(94.6951647367994,0.504807599149018,1.7030700456644));
#23432=CARTESIAN_POINT('Ctrl Pts',(94.696976590368,0.478642792623929,1.71059159168385));
#23433=CARTESIAN_POINT('Ctrl Pts',(94.69781848405,0.466508543641666,1.71394057105261));
#23434=CARTESIAN_POINT('Ctrl Pts',(94.699706668907,0.439353296001084,1.72112552370746));
#23435=CARTESIAN_POINT('Ctrl Pts',(94.7007550619951,0.424315764836678,1.7248943423168));
#23436=CARTESIAN_POINT('Ctrl Pts',(94.7038435006594,0.380147020980542,1.73535172607837));
#23437=CARTESIAN_POINT('Ctrl Pts',(94.7059004526027,0.350895278964155,1.74150213484107));
#23438=CARTESIAN_POINT('Ctrl Pts',(94.7176422025601,0.184928678780679,1.77204683817166));
#23439=CARTESIAN_POINT('Ctrl Pts',(94.7278036701228,0.0458971188206476,
1.78107527401617));
#23440=CARTESIAN_POINT('Ctrl Pts',(94.7433518483741,-0.166687648977784,
1.76996133130152));
#23441=CARTESIAN_POINT('Ctrl Pts',(94.7487277392569,-0.240332713673877,
1.7614738598405));
#23442=CARTESIAN_POINT('Ctrl Pts',(94.7551796988284,-0.330905801390029,
1.74524713219039));
#23443=CARTESIAN_POINT('Ctrl Pts',(94.7564269756732,-0.348524627389978,
1.7418142403167));
#23444=CARTESIAN_POINT('Ctrl Pts',(94.7582661572736,-0.37471092852178,1.73629876869733));
#23445=CARTESIAN_POINT('Ctrl Pts',(94.7588683888926,-0.383319246085154,
1.73441865131664));
#23446=CARTESIAN_POINT('Ctrl Pts',(94.7599015200691,-0.398151335312461,
1.73106339548803));
#23447=CARTESIAN_POINT('Ctrl Pts',(94.7603340780327,-0.404381504539101,
1.72961861906444));
#23448=CARTESIAN_POINT('Ctrl Pts',(94.7613480160721,-0.419032773200892,
1.7261374948814));
#23449=CARTESIAN_POINT('Ctrl Pts',(94.7619277994183,-0.427446939058697,
1.72407315343835));
#23450=CARTESIAN_POINT('Ctrl Pts',(94.7636483532449,-0.452512394625666,
1.71772878054635));
#23451=CARTESIAN_POINT('Ctrl Pts',(94.7647794519678,-0.46911754416834,1.71326834279269));
#23452=CARTESIAN_POINT('Ctrl Pts',(94.7747314778119,-0.616043624103585,
1.67150496569941));
#23453=CARTESIAN_POINT('Ctrl Pts',(94.7828789277683,-0.741778709836186,
1.61963376317424));
#23454=CARTESIAN_POINT('Ctrl Pts',(94.7965158145034,-0.935389078075606,
1.51243458815743));
#23455=CARTESIAN_POINT('Ctrl Pts',(94.8018566878511,-1.00726520876277,1.46554614518653));
#23456=CARTESIAN_POINT('Ctrl Pts',(94.8090609716115,-1.09613288996187,1.39793802118573));
#23457=CARTESIAN_POINT('Ctrl Pts',(94.8107516775684,-1.11644616710133,1.38176910774818));
#23458=CARTESIAN_POINT('Ctrl Pts',(94.8134162119841,-1.14756491146864,1.35586503121801));
#23459=CARTESIAN_POINT('Ctrl Pts',(94.8143778503374,-1.15861803226294,1.34643211604601));
#23460=CARTESIAN_POINT('Ctrl Pts',(94.8161835747475,-1.17903424494436,1.32857102805436));
#23461=CARTESIAN_POINT('Ctrl Pts',(94.817026217257,-1.18842587279467,1.3201767525964));
#23462=CARTESIAN_POINT('Ctrl Pts',(94.8189247595603,-1.20927795213504,1.30113625739842));
#23463=CARTESIAN_POINT('Ctrl Pts',(94.8199828696199,-1.22068852365681,1.29043722307731));
#23464=CARTESIAN_POINT('Ctrl Pts',(94.823199919638,-1.25473719743749,1.25765602384183));
#23465=CARTESIAN_POINT('Ctrl Pts',(94.8253784186078,-1.27692724192742,1.23511971288841));
#23466=CARTESIAN_POINT('Ctrl Pts',(94.8371486320243,-1.39217754394153,1.11164421747947));
#23467=CARTESIAN_POINT('Ctrl Pts',(94.8471985692515,-1.47388785594181,1.00077644812121));
#23468=CARTESIAN_POINT('Ctrl Pts',(94.8625932444726,-1.5785141985714,0.81778177198603));
#23469=CARTESIAN_POINT('Ctrl Pts',(94.8679314715715,-1.61102415379445,0.75171626176366));
#23470=CARTESIAN_POINT('Ctrl Pts',(94.8743441197914,-1.64623516857952,0.667303579986147));
#23471=CARTESIAN_POINT('Ctrl Pts',(94.8755876235366,-1.65287477653436,0.650683742359493));
#23472=CARTESIAN_POINT('Ctrl Pts',(94.8774223810441,-1.6624034365569,0.625744618659666));
#23473=CARTESIAN_POINT('Ctrl Pts',(94.8780238922851,-1.66548343523797,0.617500161052013));
#23474=CARTESIAN_POINT('Ctrl Pts',(94.8790562658407,-1.67069552866741,0.60322583606297));
#23475=CARTESIAN_POINT('Ctrl Pts',(94.8794887784543,-1.67285647035351,0.597206992577164));
#23476=CARTESIAN_POINT('Ctrl Pts',(94.8805032981934,-1.67787150806881,0.582997842207014));
#23477=CARTESIAN_POINT('Ctrl Pts',(94.8810837006139,-1.68069818185487,0.574798148054284));
#23478=CARTESIAN_POINT('Ctrl Pts',(94.8828080409108,-1.68896401518246,0.55023799496343));
#23479=CARTESIAN_POINT('Ctrl Pts',(94.8839422436567,-1.69422534011304,0.533818177735953));
#23480=CARTESIAN_POINT('Ctrl Pts',(94.8938805171768,-1.73865437172299,0.387882644196613));
#23481=CARTESIAN_POINT('Ctrl Pts',(94.902014146064,-1.76314815696876,0.254344395044266));
#23482=CARTESIAN_POINT('Ctrl Pts',(94.9156436470429,-1.77800514207434,0.0336474295589285));
#23483=CARTESIAN_POINT('Ctrl Pts',(94.9209925513435,-1.77755341266031,-0.0523057006092893));
#23484=CARTESIAN_POINT('Ctrl Pts',(94.9282066195989,-1.76887356874582,-0.163784232731389));
#23485=CARTESIAN_POINT('Ctrl Pts',(94.9298984905342,-1.76628901444982,-0.189636446748442));
#23486=CARTESIAN_POINT('Ctrl Pts',(94.9325644519211,-1.76137581294171,-0.229849002382516));
#23487=CARTESIAN_POINT('Ctrl Pts',(94.9335263302914,-1.75943609631714,-0.244253802762519));
#23488=CARTESIAN_POINT('Ctrl Pts',(94.9353322685,-1.75548583193232,-0.271094471967802));
#23489=CARTESIAN_POINT('Ctrl Pts',(94.936174881674,-1.75351933468391,-0.283535972364107));
#23490=CARTESIAN_POINT('Ctrl Pts',(94.9380730438232,-1.74881538227752,-0.311373289543897));
#23491=CARTESIAN_POINT('Ctrl Pts',(94.9391307991114,-1.74600663579744,-0.326755821928492));
#23492=CARTESIAN_POINT('Ctrl Pts',(94.9418685414967,-1.73825985605987,-0.366225701290413));
#23493=CARTESIAN_POINT('Ctrl Pts',(94.9435578059455,-1.73302424047215,-0.390250519812725));
#23494=CARTESIAN_POINT('Ctrl Pts',(94.9527680006219,-1.7020518113678,-0.519424495736892));
#23495=CARTESIAN_POINT('Ctrl Pts',(94.9605724882779,-1.66724583457143,-0.622146704862753));
#23496=CARTESIAN_POINT('Ctrl Pts',(94.974367684127,-1.59057497328718,-0.794758207532667));
#23497=CARTESIAN_POINT('Ctrl Pts',(94.9802926039962,-1.55285040567036,-0.866155782714915));
#23498=CARTESIAN_POINT('Ctrl Pts',(94.9880073159767,-1.49628592561781,-0.957555286424896));
#23499=CARTESIAN_POINT('Ctrl Pts',(94.9899162743357,-1.48165312034302,-0.980044836723818));
#23500=CARTESIAN_POINT('Ctrl Pts',(94.9931533013092,-1.45565689703463,-1.01808519292341));
#23501=CARTESIAN_POINT('Ctrl Pts',(94.994492842988,-1.44453996153129,-1.03379825722877));
#23502=CARTESIAN_POINT('Ctrl Pts',(94.9964397486736,-1.42781948624641,-1.05663502960754));
#23503=CARTESIAN_POINT('Ctrl Pts',(94.9970591987383,-1.42241374574719,-1.06390094275559));
#23504=CARTESIAN_POINT('Ctrl Pts',(94.9981576510761,-1.41266995073597,-1.07679065208204));
#23505=CARTESIAN_POINT('Ctrl Pts',(94.998638053301,-1.40835347291731,-1.08243013565885));
#23506=CARTESIAN_POINT('Ctrl Pts',(94.9997074858732,-1.39862074363402,-1.09498917058392));
#23507=CARTESIAN_POINT('Ctrl Pts',(95.000295274383,-1.39318685066819,-1.10189458457978));
#23508=CARTESIAN_POINT('Ctrl Pts',(95.0020651534556,-1.37657646585032,-1.12268381733121));
#23509=CARTESIAN_POINT('Ctrl Pts',(95.0032367308741,-1.36524166833001,-1.13644048090984));
#23510=CARTESIAN_POINT('Ctrl Pts',(95.0108826985627,-1.2891760582864,-1.22597777126111));
#23511=CARTESIAN_POINT('Ctrl Pts',(95.0169994641277,-1.2183644697619,-1.29637551331948));
#23512=CARTESIAN_POINT('Ctrl Pts',(95.0300658645749,-1.0553379670686,-1.43322429567392));
#23513=CARTESIAN_POINT('Ctrl Pts',(95.0369961053692,-0.961918135203206,
-1.49752473354187));
#23514=CARTESIAN_POINT('Ctrl Pts',(95.0462086088977,-0.836446750404447,
-1.56727323021065));
#23515=CARTESIAN_POINT('Ctrl Pts',(95.0481806636035,-0.809497967192792,
-1.58136061964472));
#23516=CARTESIAN_POINT('Ctrl Pts',(95.0511886401256,-0.768365006204602,
-1.60153576569975));
#23517=CARTESIAN_POINT('Ctrl Pts',(95.0522065446111,-0.754440490662853,
-1.60814213072127));
#23518=CARTESIAN_POINT('Ctrl Pts',(95.0540669880168,-0.728994119532401,
-1.61981171086659));
#23519=CARTESIAN_POINT('Ctrl Pts',(95.0549073777346,-0.71750095312736,-1.6249353135456));
#23520=CARTESIAN_POINT('Ctrl Pts',(95.056739399634,-0.692455903334235,-1.63578277290479));
#23521=CARTESIAN_POINT('Ctrl Pts',(95.0577325078177,-0.678885497252915,
-1.64146121400739));
#23522=CARTESIAN_POINT('Ctrl Pts',(95.0605032897639,-0.641051475073493,
-1.65674318349393));
#23523=CARTESIAN_POINT('Ctrl Pts',(95.0622930108653,-0.616645247591543,
-1.66598123708717));
#23524=CARTESIAN_POINT('Ctrl Pts',(95.0730933858475,-0.469622138465437,
-1.71795801730542));
#23525=CARTESIAN_POINT('Ctrl Pts',(95.082527600122,-0.342842554481391,-1.74767621850269));
#23526=CARTESIAN_POINT('Ctrl Pts',(95.0968351122339,-0.148639526316249,
-1.771243377563));
#23527=CARTESIAN_POINT('Ctrl Pts',(95.1016452476878,-0.0829016188780032,
-1.77553513690401));
#23528=CARTESIAN_POINT('Ctrl Pts',(95.1088803682046,0.018248092511334,-1.77650748810208));
#23529=CARTESIAN_POINT('Ctrl Pts',(95.1113757133304,0.0535756369804111,
-1.77579331412681));
#23530=CARTESIAN_POINT('Ctrl Pts',(95.1146089270899,0.100211261944878,-1.77345733444665));
#23531=CARTESIAN_POINT('Ctrl Pts',(95.115390678858,0.111556182644242,-1.77277986487509));
#23532=CARTESIAN_POINT('Ctrl Pts',(95.1166743824403,0.1303127019245,-1.77147903212851));
#23533=CARTESIAN_POINT('Ctrl Pts',(95.1171796268895,0.137728133942607,-1.7709179341424));
#23534=CARTESIAN_POINT('Ctrl Pts',(95.1181990702182,0.152762308978348,-1.76968534737735));
#23535=CARTESIAN_POINT('Ctrl Pts',(95.1187131189579,0.160380628599035,-1.76901119592714));
#23536=CARTESIAN_POINT('Ctrl Pts',(95.1200506358053,0.180293038374202,-1.76711943600794));
#23537=CARTESIAN_POINT('Ctrl Pts',(95.120869845049,0.192579444904708,-1.76582271462945));
#23538=CARTESIAN_POINT('Ctrl Pts',(95.1244219453539,0.246192395568755,-1.75959809441629));
#23539=CARTESIAN_POINT('Ctrl Pts',(95.1270904947036,0.287355261314399,-1.75334643049213));
#23540=CARTESIAN_POINT('Ctrl Pts',(95.1358582453631,0.423887399228003,-1.72767205854021));
#23541=CARTESIAN_POINT('Ctrl Pts',(95.1417639101297,0.517877447058463,-1.70186268186232));
#23542=CARTESIAN_POINT('Ctrl Pts',(95.1532813190233,0.693661360920024,-1.63767111837042));
#23543=CARTESIAN_POINT('Ctrl Pts',(95.1588645057114,0.775569632689215,-1.60050676355487));
#23544=CARTESIAN_POINT('Ctrl Pts',(95.1663639452536,0.877549467464063,-1.54456257197392));
#23545=CARTESIAN_POINT('Ctrl Pts',(95.1680892110031,0.900498650895542,-1.5312964007958));
#23546=CARTESIAN_POINT('Ctrl Pts',(95.170796064066,0.935650901496785,-1.50991252943625));
#23547=CARTESIAN_POINT('Ctrl Pts',(95.1717648018356,0.948065412295002,-1.50214859732688));
#23548=CARTESIAN_POINT('Ctrl Pts',(95.173576938257,0.970971200338317,-1.48742644738552));
#23549=CARTESIAN_POINT('Ctrl Pts',(95.1744188017162,0.981487298961055,-1.48050841813491));
#23550=CARTESIAN_POINT('Ctrl Pts',(95.1763065340125,1.00478361710157,-1.4648256142169));
#23551=CARTESIAN_POINT('Ctrl Pts',(95.177354499995,1.01752431634909,-1.45600427070553));
#23552=CARTESIAN_POINT('Ctrl Pts',(95.1804404186302,1.05447138132665,-1.42970125183312));
#23553=CARTESIAN_POINT('Ctrl Pts',(95.1824952360227,1.07835328086762,-1.41177532823949));
#23554=CARTESIAN_POINT('Ctrl Pts',(95.1942369837869,1.21072528030964,-1.30709714128217));
#23555=CARTESIAN_POINT('Ctrl Pts',(95.2044009906684,1.30918069391501,-1.20846663201697));
#23556=CARTESIAN_POINT('Ctrl Pts',(95.2199526612276,1.44096817837964,-1.04123017214328));
#23557=CARTESIAN_POINT('Ctrl Pts',(95.2253294047492,1.4831311357932,-0.980241645017451));
#23558=CARTESIAN_POINT('Ctrl Pts',(95.2317822538845,1.53063028422761,-0.901419534870109));
#23559=CARTESIAN_POINT('Ctrl Pts',(95.2330296158846,1.53966159011307,-0.88590546597093));
#23560=CARTESIAN_POINT('Ctrl Pts',(95.2348688973155,1.55277350644968,-0.86257529287212));
#23561=CARTESIAN_POINT('Ctrl Pts',(95.2354711451779,1.55703332861872,-0.854861930429322));
#23562=CARTESIAN_POINT('Ctrl Pts',(95.2365042934527,1.56428579601105,-0.841495640838743));
#23563=CARTESIAN_POINT('Ctrl Pts',(95.2369368524538,1.56730549488526,-0.835857915242681));
#23564=CARTESIAN_POINT('Ctrl Pts',(95.2379507774485,1.57434391337453,-0.82254504737488));
#23565=CARTESIAN_POINT('Ctrl Pts',(95.2385305468916,1.57833701300949,-0.814856670691083));
#23566=CARTESIAN_POINT('Ctrl Pts',(95.2402510157348,1.5900855113624,-0.79182552374539));
#23567=CARTESIAN_POINT('Ctrl Pts',(95.2413820447975,1.59767484804097,-0.776398562132921));
#23568=CARTESIAN_POINT('Ctrl Pts',(95.2513343785186,1.66310620492509,-0.638371241198474));
#23569=CARTESIAN_POINT('Ctrl Pts',(95.2594821379166,1.70696831359905,-0.509617358587434));
#23570=CARTESIAN_POINT('Ctrl Pts',(95.2731191903442,1.7539539196056,-0.293353434769132));
#23571=CARTESIAN_POINT('Ctrl Pts',(95.278459884124,1.76606306780404,-0.20839727471165));
#23572=CARTESIAN_POINT('Ctrl Pts',(95.2856119107002,1.77373327222478,-0.0978113212449633));
#23573=CARTESIAN_POINT('Ctrl Pts',(95.2872495849426,1.77494044296943,-0.0726848531789911));
#23574=CARTESIAN_POINT('Ctrl Pts',(95.2889037169481,1.7756136383723,-0.0475422940788269));
#23575=CARTESIAN_POINT('Origin',(88.3562164250559,0.,0.));
#23576=CARTESIAN_POINT('',(96.1869838792616,1.77561363799551,-0.0475423081512957));
#23577=CARTESIAN_POINT('',(96.0403469426785,1.77561363837197,-0.0475422940912404));
#23578=CARTESIAN_POINT('',(88.3562164250559,1.77561363837197,-0.0475422940912398));
#23579=CARTESIAN_POINT('Ctrl Pts',(96.1869838792615,1.77561363799551,-0.0475423081512961));
#23580=CARTESIAN_POINT('Ctrl Pts',(96.1857088353678,1.7751328526159,-0.0654987160368496));
#23581=CARTESIAN_POINT('Ctrl Pts',(96.1844438750254,1.77438015889208,-0.0834375888448888));
#23582=CARTESIAN_POINT('Ctrl Pts',(96.1823242676866,1.77264711549215,-0.113754459212563));
#23583=CARTESIAN_POINT('Ctrl Pts',(96.1814642388469,1.7718096344516,-0.126128954223985));
#23584=CARTESIAN_POINT('Ctrl Pts',(96.1801014018478,1.77026563326307,-0.145871193086372));
#23585=CARTESIAN_POINT('Ctrl Pts',(96.179594454685,1.76964257776924,-0.153244801156153));
#23586=CARTESIAN_POINT('Ctrl Pts',(96.1786262717437,1.76835837252456,-0.167388763983415));
#23587=CARTESIAN_POINT('Ctrl Pts',(96.1781646595146,1.76770437146033,-0.174159677820498));
#23588=CARTESIAN_POINT('Ctrl Pts',(96.1771726197572,1.7662080619943,-0.18877329034128));
#23589=CARTESIAN_POINT('Ctrl Pts',(96.1766429424389,1.76535238795787,-0.196614408967168));
#23590=CARTESIAN_POINT('Ctrl Pts',(96.1752322386025,1.76292164292943,-0.217592250673031));
#23591=CARTESIAN_POINT('Ctrl Pts',(96.1743562844844,1.76125194886731,-0.230717804057732));
#23592=CARTESIAN_POINT('Ctrl Pts',(96.1700911093059,1.75233803313535,-0.295040694130992));
#23593=CARTESIAN_POINT('Ctrl Pts',(96.1668022704622,1.74300666365363,-0.345928356830504));
#23594=CARTESIAN_POINT('Ctrl Pts',(96.158256364338,1.71253779738013,-0.479035557129611));
#23595=CARTESIAN_POINT('Ctrl Pts',(96.153095153187,1.6877080152804,-0.56027103957452));
#23596=CARTESIAN_POINT('Ctrl Pts',(96.1423190744733,1.62466742839256,-0.723650590031361));
#23597=CARTESIAN_POINT('Ctrl Pts',(96.1367098101578,1.58579791136769,-0.805268139800113));
#23598=CARTESIAN_POINT('Ctrl Pts',(96.1291720542594,1.52763026622437,-0.906708946827627));
#23599=CARTESIAN_POINT('Ctrl Pts',(96.1274363557948,1.51384489714746,-0.929542280137061));
#23600=CARTESIAN_POINT('Ctrl Pts',(96.1247107667235,1.49163670038338,-0.964521673223268));
#23601=CARTESIAN_POINT('Ctrl Pts',(96.1237338599332,1.4835671888851,-0.97688816042699));
#23602=CARTESIAN_POINT('Ctrl Pts',(96.1219048125363,1.46826268301206,-0.999715202044005));
#23603=CARTESIAN_POINT('Ctrl Pts',(96.1210542185449,1.4610676585376,-1.01020150177066));
#23604=CARTESIAN_POINT('Ctrl Pts',(96.1191444932199,1.44474527060808,-1.03345118745846));
#23605=CARTESIAN_POINT('Ctrl Pts',(96.1180831935032,1.43556023075006,-1.04617257185017));
#23606=CARTESIAN_POINT('Ctrl Pts',(96.115348639551,1.41161076741906,-1.07843350737852));
#23607=CARTESIAN_POINT('Ctrl Pts',(96.1136662769424,1.39660899903011,-1.0977918693373));
#23608=CARTESIAN_POINT('Ctrl Pts',(96.1037764626145,1.30691234909745,-1.20872172087224));
#23609=CARTESIAN_POINT('Ctrl Pts',(96.0952246837161,1.22364023582482,-1.29295158645959));
#23610=CARTESIAN_POINT('Ctrl Pts',(96.0812315507888,1.07621568013534,-1.41498738769792));
#23611=CARTESIAN_POINT('Ctrl Pts',(96.0758633937944,1.01695292066245,-1.45816226063665));
#23612=CARTESIAN_POINT('Ctrl Pts',(96.0679159264959,0.923457335295051,-1.51779687471491));
#23613=CARTESIAN_POINT('Ctrl Pts',(96.0652522124573,0.891085313177671,-1.53702577551131));
#23614=CARTESIAN_POINT('Ctrl Pts',(96.0618344193847,0.847897330361275,-1.56085572996304));
#23615=CARTESIAN_POINT('Ctrl Pts',(96.0610305016613,0.837614744475606,-1.56639779458678));
#23616=CARTESIAN_POINT('Ctrl Pts',(96.0597168119931,0.820594429445155,-1.57535579695868));
#23617=CARTESIAN_POINT('Ctrl Pts',(96.0592035111115,0.813888407638603,-1.57883082408052));
#23618=CARTESIAN_POINT('Ctrl Pts',(96.0581736768961,0.800317343292535,-1.58575383432957));
#23619=CARTESIAN_POINT('Ctrl Pts',(96.0576572399717,0.793451717333784,-1.5892002551558));
#23620=CARTESIAN_POINT('Ctrl Pts',(96.0563219647286,0.775550792809677,-1.59804127003428));
#23621=CARTESIAN_POINT('Ctrl Pts',(96.0555072874269,0.764481295950203,-1.60336624077953));
#23622=CARTESIAN_POINT('Ctrl Pts',(96.0520628307256,0.717095850921767,-1.62555863764193));
#23623=CARTESIAN_POINT('Ctrl Pts',(96.0494923109065,0.680267620898655,-1.64131162497476));
#23624=CARTESIAN_POINT('Ctrl Pts',(96.040745218903,0.551248754837021,-1.69140851032364));
#23625=CARTESIAN_POINT('Ctrl Pts',(96.0347756888385,0.456757810873997,-1.71933498580347));
#23626=CARTESIAN_POINT('Ctrl Pts',(96.0231674592808,0.272039646143258,-1.75761425798143));
#23627=CARTESIAN_POINT('Ctrl Pts',(96.0175585140702,0.182385597518182,-1.76916542651245));
#23628=CARTESIAN_POINT('Ctrl Pts',(96.0100211468007,0.0656148744643614,
-1.77523801087929));
#23629=CARTESIAN_POINT('Ctrl Pts',(96.0082854929294,0.0389550962791041,
-1.77602299707647));
#23630=CARTESIAN_POINT('Ctrl Pts',(96.0055599584461,-0.00247689172977802,
-1.77630964778879));
#23631=CARTESIAN_POINT('Ctrl Pts',(96.0045830607841,-0.0172429363623765,
-1.77622767652045));
#23632=CARTESIAN_POINT('Ctrl Pts',(96.0027540216911,-0.0447210949801193,
-1.77573247293889));
#23633=CARTESIAN_POINT('Ctrl Pts',(96.0019034267566,-0.0574331912096921,
-1.77536678064391));
#23634=CARTESIAN_POINT('Ctrl Pts',(95.9999936878182,-0.0858184153194282,
-1.77424503920926));
#23635=CARTESIAN_POINT('Ctrl Pts',(95.9989323752868,-0.101487491118157,
-1.77341775143683));
#23636=CARTESIAN_POINT('Ctrl Pts',(95.9961977646379,-0.141579742644782,
-1.77076791137351));
#23637=CARTESIAN_POINT('Ctrl Pts',(95.9945153575012,-0.16597922630481,-1.76864767885796));
#23638=CARTESIAN_POINT('Ctrl Pts',(95.9846271332759,-0.307791652030535,
-1.75336441930909));
#23639=CARTESIAN_POINT('Ctrl Pts',(95.9760771432209,-0.423681990049061,
-1.72901914652318));
#23640=CARTESIAN_POINT('Ctrl Pts',(95.9620845491921,-0.606125472792167,
-1.67124021074423));
#23641=CARTESIAN_POINT('Ctrl Pts',(95.9567151438684,-0.674539649504443,
-1.64481887017444));
#23642=CARTESIAN_POINT('Ctrl Pts',(95.9487661112058,-0.775339942739593,
-1.59853968928132));
#23643=CARTESIAN_POINT('Ctrl Pts',(95.9461020474553,-0.809045954034763,
-1.58174785486638));
#23644=CARTESIAN_POINT('Ctrl Pts',(95.9426838827033,-0.852479740646801,
-1.55835772400399));
#23645=CARTESIAN_POINT('Ctrl Pts',(95.9418799300617,-0.862709571760135,
-1.55271784862184));
#23646=CARTESIAN_POINT('Ctrl Pts',(95.9405661984831,-0.879461208110358,
-1.54326572230753));
#23647=CARTESIAN_POINT('Ctrl Pts',(95.9400528901852,-0.886015501941521,
-1.53951214449439));
#23648=CARTESIAN_POINT('Ctrl Pts',(95.9390857932915,-0.89838490517734,-1.53232314997505));
#23649=CARTESIAN_POINT('Ctrl Pts',(95.9386314572816,-0.904204690934587,
-1.52889618828624));
#23650=CARTESIAN_POINT('Ctrl Pts',(95.9374154093264,-0.919800049902042,
-1.51959271514326));
#23651=CARTESIAN_POINT('Ctrl Pts',(95.9366575498323,-0.929538999700365,
-1.5136549860434));
#23652=CARTESIAN_POINT('Ctrl Pts',(95.9337711848109,-0.966671608829576,
-1.49052208848886));
#23653=CARTESIAN_POINT('Ctrl Pts',(95.9316806273558,-0.993652654860034,
-1.47267267332686));
#23654=CARTESIAN_POINT('Ctrl Pts',(95.922978621307,-1.10546082279982,-1.39423267999788));
#23655=CARTESIAN_POINT('Ctrl Pts',(95.9166532067125,-1.18536097272046,-1.3269707881487));
#23656=CARTESIAN_POINT('Ctrl Pts',(95.9045081739203,-1.3246962871328,-1.18698816532649));
#23657=CARTESIAN_POINT('Ctrl Pts',(95.8987241485187,-1.38517230602763,-1.11582079992327));
#23658=CARTESIAN_POINT('Ctrl Pts',(95.8909735744636,-1.45562086892164,-1.01831413005185));
#23659=CARTESIAN_POINT('Ctrl Pts',(95.8892137637703,-1.4709589032715,-0.99602989916447));
#23660=CARTESIAN_POINT('Ctrl Pts',(95.8864586657417,-1.49391587479961,-0.960988943519251));
#23661=CARTESIAN_POINT('Ctrl Pts',(95.8854768344005,-1.50189408401975,-0.948471680371219));
#23662=CARTESIAN_POINT('Ctrl Pts',(95.8836432665788,-1.5164120336636,-0.925051462949214));
#23663=CARTESIAN_POINT('Ctrl Pts',(95.8827931405099,-1.52299344540297,-0.914175374698735));
#23664=CARTESIAN_POINT('Ctrl Pts',(95.8808905592942,-1.53738687335471,-0.889802690713056));
#23665=CARTESIAN_POINT('Ctrl Pts',(95.8798360119085,-1.54513895298242,-0.876272112787254));
#23666=CARTESIAN_POINT('Ctrl Pts',(95.8771312793624,-1.56444365498687,-0.841524615788146));
#23667=CARTESIAN_POINT('Ctrl Pts',(95.8754723227704,-1.57574309682466,-0.820171458642281));
#23668=CARTESIAN_POINT('Ctrl Pts',(95.865071745911,-1.64322433047897,-0.686103649839787));
#23669=CARTESIAN_POINT('Ctrl Pts',(95.855932688856,-1.68771201773955,-0.567927819327141));
#23670=CARTESIAN_POINT('Ctrl Pts',(95.8417490813277,-1.73641358040554,-0.380211418463635));
#23671=CARTESIAN_POINT('Ctrl Pts',(95.8367726781835,-1.74970222175556,-0.313426044512158));
#23672=CARTESIAN_POINT('Ctrl Pts',(95.8293202086395,-1.76412474150759,-0.210308541965244));
#23673=CARTESIAN_POINT('Ctrl Pts',(95.8267698716343,-1.76803291358761,-0.174429987414859));
#23674=CARTESIAN_POINT('Ctrl Pts',(95.8234729399174,-1.77174328085655,-0.126974079396582));
#23675=CARTESIAN_POINT('Ctrl Pts',(95.8226806255155,-1.77252925621433,-0.115484733596155));
#23676=CARTESIAN_POINT('Ctrl Pts',(95.8213808444063,-1.77364361343896,-0.0964827459219574));
#23677=CARTESIAN_POINT('Ctrl Pts',(95.8208699891774,-1.77403612041142,-0.0889743681321824));
#23678=CARTESIAN_POINT('Ctrl Pts',(95.8198398880211,-1.77473515909593,-0.0737483946756312));
#23679=CARTESIAN_POINT('Ctrl Pts',(95.8193207894074,-1.77503905265561,-0.0660308862593962));
#23680=CARTESIAN_POINT('Ctrl Pts',(95.8179703128861,-1.77570210583479,-0.0458442284910022));
#23681=CARTESIAN_POINT('Ctrl Pts',(95.8171432743464,-1.77598027968316,-0.0333725939401568));
#23682=CARTESIAN_POINT('Ctrl Pts',(95.813549365582,-1.77662292201165,0.021244119641939));
#23683=CARTESIAN_POINT('Ctrl Pts',(95.8108484098556,-1.77561877165931,0.0633949461116137));
#23684=CARTESIAN_POINT('Ctrl Pts',(95.8020813766487,-1.76736554275527,0.202139892270353));
#23685=CARTESIAN_POINT('Ctrl Pts',(95.7962035681913,-1.75371967524114,0.298179634677757));
#23686=CARTESIAN_POINT('Ctrl Pts',(95.785292447043,-1.71453330414794,0.471071410675169));
#23687=CARTESIAN_POINT('Ctrl Pts',(95.7802986229555,-1.69144982642376,0.548204695159838));
#23688=CARTESIAN_POINT('Ctrl Pts',(95.7730926859472,-1.65195983692871,0.653545779987085));
#23689=CARTESIAN_POINT('Ctrl Pts',(95.7710148279853,-1.63988668098069,0.683275096808986));
#23690=CARTESIAN_POINT('Ctrl Pts',(95.767872295538,-1.62066802240979,0.72715165616608));
#23691=CARTESIAN_POINT('Ctrl Pts',(95.7668280295796,-1.61412718479698,0.741557667491839));
#23692=CARTESIAN_POINT('Ctrl Pts',(95.764931849606,-1.60197973373417,0.767389686379089));
#23693=CARTESIAN_POINT('Ctrl Pts',(95.7640823291062,-1.59644104046476,0.778846575315385));
#23694=CARTESIAN_POINT('Ctrl Pts',(95.7622443094546,-1.58425437049338,0.803378669922324));
#23695=CARTESIAN_POINT('Ctrl Pts',(95.7612544636352,-1.57756661614441,0.816432940798284));
#23696=CARTESIAN_POINT('Ctrl Pts',(95.7585291912953,-1.55881944883748,0.851936226078057));
#23697=CARTESIAN_POINT('Ctrl Pts',(95.7567825024734,-1.54643780892014,0.87421015381732));
#23698=CARTESIAN_POINT('Ctrl Pts',(95.7450241734097,-1.46071040510407,1.02090582666248));
#23699=CARTESIAN_POINT('Ctrl Pts',(95.7344729536275,-1.37291393775626,1.13622862133275));
#23700=CARTESIAN_POINT('Ctrl Pts',(95.7183986448979,-1.219367518874,1.29380380818812));
#23701=CARTESIAN_POINT('Ctrl Pts',(95.7129027913528,-1.16316742806164,1.34455536621618));
#23702=CARTESIAN_POINT('Ctrl Pts',(95.7063203577418,-1.08964929001053,1.40287535192581));
#23703=CARTESIAN_POINT('Ctrl Pts',(95.705056114969,-1.07522756662815,1.41395918343043));
#23704=CARTESIAN_POINT('Ctrl Pts',(95.7031934580536,-1.0534910329906,1.43013988049136));
#23705=CARTESIAN_POINT('Ctrl Pts',(95.7025844425084,-1.04630448431426,1.43540599450567));
#23706=CARTESIAN_POINT('Ctrl Pts',(95.7015400961272,-1.03383781301543,1.44439786437568));
#23707=CARTESIAN_POINT('Ctrl Pts',(95.7011030674611,-1.02857666156881,1.44814911844296));
#23708=CARTESIAN_POINT('Ctrl Pts',(95.7000784966573,-1.01613804981689,1.45691598604226));
#23709=CARTESIAN_POINT('Ctrl Pts',(95.699492586269,-1.00894383613061,1.46190733985422));
#23710=CARTESIAN_POINT('Ctrl Pts',(95.697788036691,-0.987787033792288,1.47635537900139));
#23711=CARTESIAN_POINT('Ctrl Pts',(95.6966784986424,-0.973725903815361,
1.48566696951904));
#23712=CARTESIAN_POINT('Ctrl Pts',(95.6882267718352,-0.86458844862292,1.55572493940772));
#23713=CARTESIAN_POINT('Ctrl Pts',(95.6813523267443,-0.764038928621692,
1.60749640850409));
#23714=CARTESIAN_POINT('Ctrl Pts',(95.667498007156,-0.554481991437766,1.69125469372554));
#23715=CARTESIAN_POINT('Ctrl Pts',(95.6605430926195,-0.445981092520281,
1.72304653740317));
#23716=CARTESIAN_POINT('Ctrl Pts',(95.6517109121644,-0.311962272368679,
1.74880067202562));
#23717=CARTESIAN_POINT('Ctrl Pts',(95.6501658080794,-0.288633266760026,
1.75280204270756));
#23718=CARTESIAN_POINT('Ctrl Pts',(95.6476738186553,-0.251245585136907,
1.75844812363736));
#23719=CARTESIAN_POINT('Ctrl Pts',(95.6467364491784,-0.237234649738997,
1.76039309501794));
#23720=CARTESIAN_POINT('Ctrl Pts',(95.6449400323858,-0.210493808185803,
1.76378017804981));
#23721=CARTESIAN_POINT('Ctrl Pts',(95.6440819941082,-0.197768557752873,
1.76525231693797));
#23722=CARTESIAN_POINT('Ctrl Pts',(95.6421155307026,-0.168719434020354,
1.76829486450532));
#23723=CARTESIAN_POINT('Ctrl Pts',(95.6410044038167,-0.152387711550758,
1.76977708457753));
#23724=CARTESIAN_POINT('Ctrl Pts',(95.6374089023799,-0.09981889961668,1.77381505042585));
#23725=CARTESIAN_POINT('Ctrl Pts',(95.6348973814402,-0.063525191819601,
1.77548524671327));
#23726=CARTESIAN_POINT('Ctrl Pts',(95.6231038350541,0.104856772634574,1.77806476654996));
#23727=CARTESIAN_POINT('Ctrl Pts',(95.6134218673755,0.236718578700988,1.7653507731331));
#23728=CARTESIAN_POINT('Ctrl Pts',(95.5985429796091,0.436147228549847,1.72336559272204));
#23729=CARTESIAN_POINT('Ctrl Pts',(95.5933395357185,0.505413324934643,1.70433937581619));
#23730=CARTESIAN_POINT('Ctrl Pts',(95.5870624641416,0.590165793088469,1.67543555114067));
#23731=CARTESIAN_POINT('Ctrl Pts',(95.5858276220592,0.606901412779942,1.66944622096831));
#23732=CARTESIAN_POINT('Ctrl Pts',(95.5839994542171,0.631812225563644,1.66010702244092));
#23733=CARTESIAN_POINT('Ctrl Pts',(95.5833960685007,0.640056364220105,1.65694594761901));
#23734=CARTESIAN_POINT('Ctrl Pts',(95.5823087803806,0.654958849483811,1.65110401824517));
#23735=CARTESIAN_POINT('Ctrl Pts',(95.5818237222529,0.661624816911754,1.64844416927022));
#23736=CARTESIAN_POINT('Ctrl Pts',(95.5807213507672,0.676813498223356,1.64227661520591));
#23737=CARTESIAN_POINT('Ctrl Pts',(95.5801055890829,0.685325247178726,1.63874290453633));
#23738=CARTESIAN_POINT('Ctrl Pts',(95.5781767647745,0.712059049960596,1.62739945507824));
#23739=CARTESIAN_POINT('Ctrl Pts',(95.5768770499164,0.730178778358473,1.61935052067257));
#23740=CARTESIAN_POINT('Ctrl Pts',(95.5670202812097,0.868016880735461,1.55533742030664));
#23741=CARTESIAN_POINT('Ctrl Pts',(95.5590722976478,0.981302431900621,1.48646647756767));
#23742=CARTESIAN_POINT('Ctrl Pts',(95.5471334822186,1.1346001753285,1.36803957326225));
#23743=CARTESIAN_POINT('Ctrl Pts',(95.5433111014641,1.18130134629904,1.32792173966354));
#23744=CARTESIAN_POINT('Ctrl Pts',(95.5367914287634,1.25563475894926,1.25703705903914));
#23745=CARTESIAN_POINT('Ctrl Pts',(95.5341422734579,1.28444510922151,1.22758346575362));
#23746=CARTESIAN_POINT('Ctrl Pts',(95.5303137582553,1.32390746776737,1.18432875825583));
#23747=CARTESIAN_POINT('Ctrl Pts',(95.5291708018469,1.33542174283353,1.17133015169096));
#23748=CARTESIAN_POINT('Ctrl Pts',(95.5271644550749,1.3551583480396,1.14837993674027));
#23749=CARTESIAN_POINT('Ctrl Pts',(95.5263046860705,1.3634663318484,1.13850348011373));
#23750=CARTESIAN_POINT('Ctrl Pts',(95.5245137057603,1.38045893542429,1.11785004956742));
#23751=CARTESIAN_POINT('Ctrl Pts',(95.5235818915888,1.38912666775141,1.10706038126636));
#23752=CARTESIAN_POINT('Ctrl Pts',(95.5211412928642,1.41137427847528,1.07869367359434));
#23753=CARTESIAN_POINT('Ctrl Pts',(95.5196246701492,1.42475174350624,1.06096172722781));
#23754=CARTESIAN_POINT('Ctrl Pts',(95.5121583516474,1.488414479755,0.973200273630984));
#23755=CARTESIAN_POINT('Ctrl Pts',(95.5060301775853,1.53388114915522,0.899833935221259));
#23756=CARTESIAN_POINT('Ctrl Pts',(95.4921639787674,1.62261690690744,0.730239192960171));
#23757=CARTESIAN_POINT('Ctrl Pts',(95.4843916851545,1.66301443226564,0.632864401789094));
#23758=CARTESIAN_POINT('Ctrl Pts',(95.4746051898091,1.70372718705269,0.503302718569362));
#23759=CARTESIAN_POINT('Ctrl Pts',(95.472419549125,1.71214324211356,0.47388361867349));
#23760=CARTESIAN_POINT('Ctrl Pts',(95.4687681982979,1.72510549850677,0.423704850839405));
#23761=CARTESIAN_POINT('Ctrl Pts',(95.4672872024097,1.73004674409583,0.403054765023951));
#23762=CARTESIAN_POINT('Ctrl Pts',(95.465172997492,1.73665430994928,0.373075699939175));
#23763=CARTESIAN_POINT('Ctrl Pts',(95.4645248216293,1.73861792765303,0.36381503815655));
#23764=CARTESIAN_POINT('Ctrl Pts',(95.4633914734083,1.74194294042276,0.347491835791105));
#23765=CARTESIAN_POINT('Ctrl Pts',(95.4629046089788,1.74333560496434,0.340436129825559));
#23766=CARTESIAN_POINT('Ctrl Pts',(95.4618390161632,1.74630494913922,0.324896206123856));
#23767=CARTESIAN_POINT('Ctrl Pts',(95.4612613393909,1.74786270369423,0.316408749828724));
#23768=CARTESIAN_POINT('Ctrl Pts',(95.4596042938894,1.75217779793138,0.291892996066376));
#23769=CARTESIAN_POINT('Ctrl Pts',(95.4585332800772,1.75477702331477,0.275837272882306));
#23770=CARTESIAN_POINT('Ctrl Pts',(95.4507634051892,1.77219199933964,0.158027365034681));
#23771=CARTESIAN_POINT('Ctrl Pts',(95.4444585957157,1.77836486843091,0.0552108353318123));
#23772=CARTESIAN_POINT('Ctrl Pts',(95.4381488398588,1.77561363782069,-0.0475423146804777));
#23773=CARTESIAN_POINT('Ctrl Pts',(95.2889037169481,1.7756136383723,-0.0475422940788269));
#23774=CARTESIAN_POINT('Ctrl Pts',(95.2889567569751,1.77563522449855,-0.0467360936017572));
#23775=CARTESIAN_POINT('Ctrl Pts',(95.2890098138606,1.77565626160278,-0.0459298765760937));
#23776=CARTESIAN_POINT('Ctrl Pts',(95.2900191314892,1.77604588821666,-0.030597539362922));
#23777=CARTESIAN_POINT('Ctrl Pts',(95.2909807644722,1.77623675511927,-0.0160678287640855));
#23778=CARTESIAN_POINT('Ctrl Pts',(95.292786484101,1.77626023938196,0.0110584591401438));
#23779=CARTESIAN_POINT('Ctrl Pts',(95.2936291272694,1.77613715526875,0.0236541558387008));
#23780=CARTESIAN_POINT('Ctrl Pts',(95.2955276780908,1.77556092417017,0.0518857780285321));
#23781=CARTESIAN_POINT('Ctrl Pts',(95.2965857960983,1.77503517899466,0.0675190001902518));
#23782=CARTESIAN_POINT('Ctrl Pts',(95.2993251477812,1.77315133809973,0.107720967200315));
#23783=CARTESIAN_POINT('Ctrl Pts',(95.3010156772862,1.77148910383564,0.132271403366321));
#23784=CARTESIAN_POINT('Ctrl Pts',(95.3100389491564,1.76000280663643,0.26189966955908));
#23785=CARTESIAN_POINT('Ctrl Pts',(95.317639745967,1.74133979125052,0.365965209429774));
#23786=CARTESIAN_POINT('Ctrl Pts',(95.3313800827805,1.69178020528202,0.54752442454029));
#23787=CARTESIAN_POINT('Ctrl Pts',(95.3374587743909,1.66445716285109,0.625688772466514));
#23788=CARTESIAN_POINT('Ctrl Pts',(95.3453486436257,1.62105031371086,0.726635141924815));
#23789=CARTESIAN_POINT('Ctrl Pts',(95.3472834545113,1.60974170785838,0.751355136635535));
#23790=CARTESIAN_POINT('Ctrl Pts',(95.3505592873381,1.58938214784155,0.793288141020426));
#23791=CARTESIAN_POINT('Ctrl Pts',(95.3519121247525,1.58060791319242,0.810629624762761));
#23792=CARTESIAN_POINT('Ctrl Pts',(95.353874481689,1.56731387071871,0.835867170273672));
#23793=CARTESIAN_POINT('Ctrl Pts',(95.3544963506445,1.56301553476532,0.84387744540039));
#23794=CARTESIAN_POINT('Ctrl Pts',(95.3555973085542,1.55524937915512,0.85808733931189));
#23795=CARTESIAN_POINT('Ctrl Pts',(95.3560778260503,1.55180565123194,0.864299565729837));
#23796=CARTESIAN_POINT('Ctrl Pts',(95.3571453502307,1.54403351899381,0.878123693241679));
#23797=CARTESIAN_POINT('Ctrl Pts',(95.3577311410998,1.53968599991507,0.885724425640546));
#23798=CARTESIAN_POINT('Ctrl Pts',(95.3594886364846,1.52639876248971,0.908560900650809));
#23799=CARTESIAN_POINT('Ctrl Pts',(95.3606500423319,1.51728751014733,0.923696249839533));
#23800=CARTESIAN_POINT('Ctrl Pts',(95.3704647085506,1.43761189875432,1.05169001771807));
#23801=CARTESIAN_POINT('Ctrl Pts',(95.3784742427342,1.35478459329991,1.1564378834565));
#23802=CARTESIAN_POINT('Ctrl Pts',(95.3920387478449,1.19968572964695,1.31278430215599));
#23803=CARTESIAN_POINT('Ctrl Pts',(95.397460708626,1.13389482277488,1.37001041091376));
#23804=CARTESIAN_POINT('Ctrl Pts',(95.4047637773581,1.04324417362927,1.43784186419669));
#23805=CARTESIAN_POINT('Ctrl Pts',(95.4064661838775,1.02196834910212,1.45304102179414));
#23806=CARTESIAN_POINT('Ctrl Pts',(95.4091450488351,0.988327214095373,1.47596938510215));
#23807=CARTESIAN_POINT('Ctrl Pts',(95.41010909565,0.976188565537531,1.48402566390425));
#23808=CARTESIAN_POINT('Ctrl Pts',(95.4119169751055,0.953375225851697,1.4987656002174));
#23809=CARTESIAN_POINT('Ctrl Pts',(95.4127593329812,0.942725826917928,1.50548684711106));
#23810=CARTESIAN_POINT('Ctrl Pts',(95.4146541083425,0.918733523813713,1.5202749294355));
#23811=CARTESIAN_POINT('Ctrl Pts',(95.4157086968476,0.905354201517406,1.52828037073147));
#23812=CARTESIAN_POINT('Ctrl Pts',(95.4188338191507,0.865643058637727,1.5513368422232));
#23813=CARTESIAN_POINT('Ctrl Pts',(95.4209218709622,0.839030299551189,1.56589011837562));
#23814=CARTESIAN_POINT('Ctrl Pts',(95.4326637930602,0.689018250436116,1.64300255133708));
#23815=CARTESIAN_POINT('Ctrl Pts',(95.4427884366524,0.559026885822932,1.69165001133641));
#23816=CARTESIAN_POINT('Ctrl Pts',(95.4582859577275,0.352994575201968,1.74238870317995));
#23817=CARTESIAN_POINT('Ctrl Pts',(95.4636494593696,0.280209969315898,1.755564870218));
#23818=CARTESIAN_POINT('Ctrl Pts',(95.4700884913032,0.189001250514819,1.7662570887508));
#23819=CARTESIAN_POINT('Ctrl Pts',(95.4713345295017,0.171160936196939,1.76807510357048));
#23820=CARTESIAN_POINT('Ctrl Pts',(95.4731722589091,0.144520660305005,1.77038284380619));
#23821=CARTESIAN_POINT('Ctrl Pts',(95.4737742541813,0.135740233241383,1.77107770362842));
#23822=CARTESIAN_POINT('Ctrl Pts',(95.4748071366485,0.120575778910655,1.7721643390175));
#23823=CARTESIAN_POINT('Ctrl Pts',(95.47523967959,0.114194424307764,1.77258697953274));
#23824=CARTESIAN_POINT('Ctrl Pts',(95.476253807791,0.0991600884922154,1.7735011833066));
#23825=CARTESIAN_POINT('Ctrl Pts',(95.4768337937103,0.0905056281993163,
1.77396389745605));
#23826=CARTESIAN_POINT('Ctrl Pts',(95.478555586038,0.0646582664232599,1.7751561856315));
#23827=CARTESIAN_POINT('Ctrl Pts',(95.4796876999827,0.0474572288909502,
1.77569931019369));
#23828=CARTESIAN_POINT('Ctrl Pts',(95.4896352351377,-0.10520247665701,1.77829954263295));
#23829=CARTESIAN_POINT('Ctrl Pts',(95.4977781717089,-0.240493755347008,
1.76510343682338));
#23830=CARTESIAN_POINT('Ctrl Pts',(95.5114126433726,-0.456831123819215,
1.71864017195717));
#23831=CARTESIAN_POINT('Ctrl Pts',(95.5167561370058,-0.539255165748686,
1.69458554633152));
#23832=CARTESIAN_POINT('Ctrl Pts',(95.5239636132052,-0.643949959118246,
1.65561673851572));
#23833=CARTESIAN_POINT('Ctrl Pts',(95.5256546994125,-0.668082972303091,
1.64602653817489));
#23834=CARTESIAN_POINT('Ctrl Pts',(95.5283196995966,-0.705380083268758,
1.63024973017905));
#23835=CARTESIAN_POINT('Ctrl Pts',(95.529281416297,-0.718693702021668,1.62442438610772));
#23836=CARTESIAN_POINT('Ctrl Pts',(95.5310872104721,-0.74341101328943,1.61324604133307));
#23837=CARTESIAN_POINT('Ctrl Pts',(95.5319298433819,-0.754832206891317,
1.60793378280441));
#23838=CARTESIAN_POINT('Ctrl Pts',(95.533828261477,-0.780305862201823,1.59575419011407));
#23839=CARTESIAN_POINT('Ctrl Pts',(95.5348862556368,-0.794325908626361,
1.58882188976646));
#23840=CARTESIAN_POINT('Ctrl Pts',(95.5376250578013,-0.830156982302269,
1.5705121959691));
#23841=CARTESIAN_POINT('Ctrl Pts',(95.539315155324,-0.851825866566442,1.55886553642567));
#23842=CARTESIAN_POINT('Ctrl Pts',(95.5484254009532,-0.966242777113065,
1.49427041779988));
#23843=CARTESIAN_POINT('Ctrl Pts',(95.5561207371852,-1.05430147796885,1.43349602441605));
#23844=CARTESIAN_POINT('Ctrl Pts',(95.5698862838805,-1.19918587652719,1.31289740833896));
#23845=CARTESIAN_POINT('Ctrl Pts',(95.5758932017624,-1.25833059591255,1.25632453254595));
#23846=CARTESIAN_POINT('Ctrl Pts',(95.5837013943358,-1.33155823116844,1.17590244557733));
#23847=CARTESIAN_POINT('Ctrl Pts',(95.5856242166804,-1.34928941567765,1.15551378754126));
#23848=CARTESIAN_POINT('Ctrl Pts',(95.5888820635261,-1.37890838680442,1.11984373617836));
#23849=CARTESIAN_POINT('Ctrl Pts',(95.5902287441765,-1.39102395060464,1.10475824404048));
#23850=CARTESIAN_POINT('Ctrl Pts',(95.5921839484508,-1.40845705758532,1.08231008662252));
#23851=CARTESIAN_POINT('Ctrl Pts',(95.5928046992405,-1.41396804478474,1.0751003599824));
#23852=CARTESIAN_POINT('Ctrl Pts',(95.5939044971344,-1.42369348697048,1.0621729430886));
#23853=CARTESIAN_POINT('Ctrl Pts',(95.5943849595714,-1.42792918040901,1.05647184856721));
#23854=CARTESIAN_POINT('Ctrl Pts',(95.5954533580801,-1.43731874894874,1.04367417808829));
#23855=CARTESIAN_POINT('Ctrl Pts',(95.596040066375,-1.44245438550155,1.03656467717824));
#23856=CARTESIAN_POINT('Ctrl Pts',(95.5978032427166,-1.45781674004315,1.014962570548));
#23857=CARTESIAN_POINT('Ctrl Pts',(95.5989693139755,-1.46787958669407,1.00035405976913));
#23858=CARTESIAN_POINT('Ctrl Pts',(95.6087621676403,-1.55136118722488,0.875188621493969));
#23859=CARTESIAN_POINT('Ctrl Pts',(95.616749833043,-1.61240478340171,0.756860218467986));
#23860=CARTESIAN_POINT('Ctrl Pts',(95.6303031327307,-1.69080498883349,0.551240022642908));
#23861=CARTESIAN_POINT('Ctrl Pts',(95.635738147226,-1.71585017495635,0.467485571504157));
#23862=CARTESIAN_POINT('Ctrl Pts',(95.6430571171658,-1.74026808789838,0.356673740675966));
#23863=CARTESIAN_POINT('Ctrl Pts',(95.644761394455,-1.74533472498702,0.330992081121534));
#23864=CARTESIAN_POINT('Ctrl Pts',(95.6474425503943,-1.75233620935234,0.290850980786398));
#23865=CARTESIAN_POINT('Ctrl Pts',(95.6484069818381,-1.75466366536883,0.276463168926865));
#23866=CARTESIAN_POINT('Ctrl Pts',(95.6502152074162,-1.75867150712158,0.249593997069679));
#23867=CARTESIAN_POINT('Ctrl Pts',(95.6510575218129,-1.76039672802214,0.237120178823154));
#23868=CARTESIAN_POINT('Ctrl Pts',(95.6529517052858,-1.76395984030129,0.209171180553178));
#23869=CARTESIAN_POINT('Ctrl Pts',(95.6540057391991,-1.76572697637211,0.193688200059735));
#23870=CARTESIAN_POINT('Ctrl Pts',(95.6567269893385,-1.7697381345931,0.153904242847135));
#23871=CARTESIAN_POINT('Ctrl Pts',(95.6584032945087,-1.77168541033969,0.129577331701055));
#23872=CARTESIAN_POINT('Ctrl Pts',(95.6682799282808,-1.78012561000926,-0.0126552740673993));
#23873=CARTESIAN_POINT('Ctrl Pts',(95.6768242920583,-1.77534785518076,-0.13091404682957));
#23874=CARTESIAN_POINT('Ctrl Pts',(95.6908325577483,-1.7486190217658,-0.320631832753723));
#23875=CARTESIAN_POINT('Ctrl Pts',(95.6962229262214,-1.7338447082113,-0.392755283832904));
#23876=CARTESIAN_POINT('Ctrl Pts',(95.7041929795941,-1.70480804625936,-0.500111891028008));
#23877=CARTESIAN_POINT('Ctrl Pts',(95.7068580308758,-1.69382078244656,-0.536147370772488));
#23878=CARTESIAN_POINT('Ctrl Pts',(95.7102722677517,-1.6779569328271,-0.582803086805409));
#23879=CARTESIAN_POINT('Ctrl Pts',(95.7110714577312,-1.67411088460751,-0.593760617247399));
#23880=CARTESIAN_POINT('Ctrl Pts',(95.7123760738497,-1.66760841364111,-0.611720779228909));
#23881=CARTESIAN_POINT('Ctrl Pts',(95.7128850017494,-1.66501473709595,-0.618745557040854));
#23882=CARTESIAN_POINT('Ctrl Pts',(95.7139040863731,-1.65970411830595,-0.632853736697608));
#23883=CARTESIAN_POINT('Ctrl Pts',(95.7144141683819,-1.65698607423378,-0.639936534062021));
#23884=CARTESIAN_POINT('Ctrl Pts',(95.7157290334178,-1.6498264013224,-0.658242034933834));
#23885=CARTESIAN_POINT('Ctrl Pts',(95.7165298199042,-1.6453155323066,-0.669437487859746));
#23886=CARTESIAN_POINT('Ctrl Pts',(95.7198650187112,-1.62591156038618,-0.716214669699074));
#23887=CARTESIAN_POINT('Ctrl Pts',(95.7223444979818,-1.60997452978397,-0.7513550160481));
#23888=CARTESIAN_POINT('Ctrl Pts',(95.7336227994741,-1.53112981094059,-0.911151326632204));
#23889=CARTESIAN_POINT('Ctrl Pts',(95.7419603957487,-1.45480748555993,-1.02863789231543));
#23890=CARTESIAN_POINT('Ctrl Pts',(95.7546477826124,-1.32482782509322,-1.18488034935258));
#23891=CARTESIAN_POINT('Ctrl Pts',(95.7586811772971,-1.28155381786269,-1.23155540312163));
#23892=CARTESIAN_POINT('Ctrl Pts',(95.7641204709636,-1.22151773540648,-1.28971235158172));
#23893=CARTESIAN_POINT('Ctrl Pts',(95.7654308678538,-1.20692898869114,-1.30337480831913));
#23894=CARTESIAN_POINT('Ctrl Pts',(95.7676300889238,-1.18226136993859,-1.32570687810135));
#23895=CARTESIAN_POINT('Ctrl Pts',(95.7685129864217,-1.17230990650838,-1.33451494568973));
#23896=CARTESIAN_POINT('Ctrl Pts',(95.7702590175617,-1.15254162724532,-1.35162015635374));
#23897=CARTESIAN_POINT('Ctrl Pts',(95.7711217948082,-1.14273172177401,-1.35992405912022));
#23898=CARTESIAN_POINT('Ctrl Pts',(95.7730348533302,-1.12089395174406,-1.37800619462187));
#23899=CARTESIAN_POINT('Ctrl Pts',(95.7740870541833,-1.10882657378586,-1.38773481836656));
#23900=CARTESIAN_POINT('Ctrl Pts',(95.7777356205297,-1.06680023153331,-1.42071798097195));
#23901=CARTESIAN_POINT('Ctrl Pts',(95.7803628946681,-1.03622664760975,-1.44316882991483));
#23902=CARTESIAN_POINT('Ctrl Pts',(95.7921189217657,-0.898136643439155,
-1.53792014364113));
#23903=CARTESIAN_POINT('Ctrl Pts',(95.8016211782258,-0.783627371509781,
-1.59930192188895));
#23904=CARTESIAN_POINT('Ctrl Pts',(95.8162594180626,-0.597602680518702,
-1.6742101222443));
#23905=CARTESIAN_POINT('Ctrl Pts',(95.8214073029766,-0.530180878403013,
-1.69676712207639));
#23906=CARTESIAN_POINT('Ctrl Pts',(95.8276207821158,-0.444567243197875,
-1.71980654548467));
#23907=CARTESIAN_POINT('Ctrl Pts',(95.8288448671336,-0.427482890095324,
-1.72413254277283));
#23908=CARTESIAN_POINT('Ctrl Pts',(95.8306568320006,-0.40182520859577,-1.73022457642646));
#23909=CARTESIAN_POINT('Ctrl Pts',(95.8312546154195,-0.393299177310323,
-1.73218253899933));
#23910=CARTESIAN_POINT('Ctrl Pts',(95.832283089745,-0.378517749760222,-1.73546225656846));
#23911=CARTESIAN_POINT('Ctrl Pts',(95.8327153889454,-0.372269336219983,
-1.73681331051157));
#23912=CARTESIAN_POINT('Ctrl Pts',(95.8337330207187,-0.357477166869674,
-1.73992822746252));
#23913=CARTESIAN_POINT('Ctrl Pts',(95.8343167064039,-0.348927549244659,
-1.74166292231038));
#23914=CARTESIAN_POINT('Ctrl Pts',(95.8360612059315,-0.323191439976269,
-1.74668759047755));
#23915=CARTESIAN_POINT('Ctrl Pts',(95.8372119438464,-0.305968200185593,
-1.74978677634062));
#23916=CARTESIAN_POINT('Ctrl Pts',(95.8470757825022,-0.156505527743785,
-1.77440693285009));
#23917=CARTESIAN_POINT('Ctrl Pts',(95.8551346510661,-0.0222519488528085,
-1.78115945505472));
#23918=CARTESIAN_POINT('Ctrl Pts',(95.86872470928,0.197921036881598,-1.76731141462302));
#23919=CARTESIAN_POINT('Ctrl Pts',(95.8741174196764,0.28382058694742,-1.75556423829484));
#23920=CARTESIAN_POINT('Ctrl Pts',(95.8813848559755,0.394026871901089,-1.7321913853027));
#23921=CARTESIAN_POINT('Ctrl Pts',(95.8830830576458,0.419414942951327,-1.72621990571574));
#23922=CARTESIAN_POINT('Ctrl Pts',(95.8857567729684,0.458752965389729,-1.71604825970502));
#23923=CARTESIAN_POINT('Ctrl Pts',(95.8867199548095,0.472798910454391,-1.71223160873554));
#23924=CARTESIAN_POINT('Ctrl Pts',(95.8885270578465,0.498907941972941,-1.70479134780101));
#23925=CARTESIAN_POINT('Ctrl Pts',(95.8893695154734,0.510982533524763,-1.70121118924979));
#23926=CARTESIAN_POINT('Ctrl Pts',(95.8912656315735,0.53793498192917,-1.6929068685143));
#23927=CARTESIAN_POINT('Ctrl Pts',(95.8923214750549,0.552790529390272,-1.68811442553147));
#23928=CARTESIAN_POINT('Ctrl Pts',(95.8950507405519,0.590789138473322,-1.67530061332203));
#23929=CARTESIAN_POINT('Ctrl Pts',(95.8967333428618,0.61383227082159,-1.66699543803297));
#23930=CARTESIAN_POINT('Ctrl Pts',(95.9063472607885,0.743293026964865,-1.61728718471595));
#23931=CARTESIAN_POINT('Ctrl Pts',(95.9145978230967,0.845678409672861,-1.56618080532499));
#23932=CARTESIAN_POINT('Ctrl Pts',(95.9285195167745,1.00712684056962,-1.46512257049888));
#23933=CARTESIAN_POINT('Ctrl Pts',(95.9341182687157,1.0691429145886,-1.42050095619035));
#23934=CARTESIAN_POINT('Ctrl Pts',(95.9414592995003,1.14821880294892,-1.35548373379674));
#23935=CARTESIAN_POINT('Ctrl Pts',(95.9433112967371,1.16797394824887,-1.33849899911817));
#23936=CARTESIAN_POINT('Ctrl Pts',(95.9464625537674,1.20135449122553,-1.30849762554876));
#23937=CARTESIAN_POINT('Ctrl Pts',(95.9477725475971,1.21515931674008,-1.29568767661392));
#23938=CARTESIAN_POINT('Ctrl Pts',(95.9496850503181,1.23524206220112,-1.27644887287705));
#23939=CARTESIAN_POINT('Ctrl Pts',(95.9502990688375,1.24167863245428,-1.27018851348149));
#23940=CARTESIAN_POINT('Ctrl Pts',(95.9513919490235,1.25311975636645,-1.25889052425667));
#23941=CARTESIAN_POINT('Ctrl Pts',(95.9518721462221,1.25814187298278,-1.25387140813795));
#23942=CARTESIAN_POINT('Ctrl Pts',(95.9529461021718,1.26936222072975,-1.24252247040516));
#23943=CARTESIAN_POINT('Ctrl Pts',(95.9535385585971,1.27554334277323,-1.23617625197792));
#23944=CARTESIAN_POINT('Ctrl Pts',(95.9553375761283,1.29427529917168,-1.21665386605456));
#23945=CARTESIAN_POINT('Ctrl Pts',(95.9565331108233,1.3066718025701,-1.20333039657947));
#23946=CARTESIAN_POINT('Ctrl Pts',(95.9633972034397,1.37736840248741,-1.12496627388031));
#23947=CARTESIAN_POINT('Ctrl Pts',(95.9687956673541,1.43101906050624,-1.05587921425144));
#23948=CARTESIAN_POINT('Ctrl Pts',(95.9793254826991,1.52583142595219,-0.913207675557202));
#23949=CARTESIAN_POINT('Ctrl Pts',(95.9844471332954,1.56727508045992,-0.840094022792539));
#23950=CARTESIAN_POINT('Ctrl Pts',(95.9934777140294,1.62940089865141,-0.709767542782186));
#23951=CARTESIAN_POINT('Ctrl Pts',(95.9973173968418,1.65260504635709,-0.653920992698155));
#23952=CARTESIAN_POINT('Ctrl Pts',(96.0025331444676,1.67953018389623,-0.578471802134207));
#23953=CARTESIAN_POINT('Ctrl Pts',(96.0038237967921,1.6858352068965,-0.559831107542047));
#23954=CARTESIAN_POINT('Ctrl Pts',(96.0059991081082,1.69585849454098,-0.52849124562871));
#23955=CARTESIAN_POINT('Ctrl Pts',(96.0068781186967,1.69974697748888,-0.515848065441243));
#23956=CARTESIAN_POINT('Ctrl Pts',(96.008623586272,1.70714797954547,-0.490791447347547));
#23957=CARTESIAN_POINT('Ctrl Pts',(96.0094897625665,1.71066719104934,-0.478380826411765));
#23958=CARTESIAN_POINT('Ctrl Pts',(96.0114193483744,1.71816656864189,-0.450792509157177));
#23959=CARTESIAN_POINT('Ctrl Pts',(96.0124848000822,1.72208138749042,-0.435598336943335));
#23960=CARTESIAN_POINT('Ctrl Pts',(96.0162287471553,1.73504945879935,-0.382357055584056));
#23961=CARTESIAN_POINT('Ctrl Pts',(96.018940331047,1.74304649795113,-0.344066903755196));
#23962=CARTESIAN_POINT('Ctrl Pts',(96.0277751294322,1.76467137305711,-0.22022774968932));
#23963=CARTESIAN_POINT('Ctrl Pts',(96.0340324368832,1.77329886426809,-0.133994673959963));
#23964=CARTESIAN_POINT('Ctrl Pts',(96.0403469426785,1.77561363837197,-0.0475422940912497));
#23965=CARTESIAN_POINT('Origin',(88.3562164250559,0.,0.));
#23966=CARTESIAN_POINT('',(96.9396785576437,1.77561363837197,-0.0475422940912381));
#23967=CARTESIAN_POINT('',(96.7921246220486,1.77561363841954,-0.0475422923145644));
#23968=CARTESIAN_POINT('',(88.3562164250559,1.77561363837197,-0.0475422940912398));
#23969=CARTESIAN_POINT('Ctrl Pts',(96.9396785576437,1.77561363837197,-0.0475422940912364));
#23970=CARTESIAN_POINT('Ctrl Pts',(96.9356232072411,1.77407956665634,-0.104836934843796));
#23971=CARTESIAN_POINT('Ctrl Pts',(96.9314956087136,1.76977293665518,-0.162037019091112));
#23972=CARTESIAN_POINT('Ctrl Pts',(96.9203869456945,1.75093773171991,-0.313679217648223));
#23973=CARTESIAN_POINT('Ctrl Pts',(96.9133474279507,1.73155256903901,-0.407312457551113));
#23974=CARTESIAN_POINT('Ctrl Pts',(96.9032963462726,1.69235891828376,-0.541227561636571));
#23975=CARTESIAN_POINT('Ctrl Pts',(96.9001618640205,1.6784100288131,-0.583049271579781));
#23976=CARTESIAN_POINT('Ctrl Pts',(96.8962234037238,1.6584755768458,-0.636146695932724));
#23977=CARTESIAN_POINT('Ctrl Pts',(96.8953517914793,1.6539061735443,-0.64793383143922));
#23978=CARTESIAN_POINT('Ctrl Pts',(96.8939565745305,1.64632941285726,-0.666876102598521));
#23979=CARTESIAN_POINT('Ctrl Pts',(96.8934285884521,1.64340041862677,-0.674061823398139));
#23980=CARTESIAN_POINT('Ctrl Pts',(96.8923965670982,1.63755149970169,-0.688146248823345));
#23981=CARTESIAN_POINT('Ctrl Pts',(96.8918923726934,1.63463486935379,-0.695046056870477));
#23982=CARTESIAN_POINT('Ctrl Pts',(96.8906286294507,1.62717751841793,-0.712381142724191));
#23983=CARTESIAN_POINT('Ctrl Pts',(96.8898724275367,1.62257989923515,-0.722791848643906));
#23984=CARTESIAN_POINT('Ctrl Pts',(96.8868220628516,1.60349758386567,-0.764901383893432));
#23985=CARTESIAN_POINT('Ctrl Pts',(96.8845728957466,1.58818052951521,-0.796217062990812));
#23986=CARTESIAN_POINT('Ctrl Pts',(96.8782783112472,1.54207879072632,-0.883839855467505));
#23987=CARTESIAN_POINT('Ctrl Pts',(96.8743160080936,1.50915069326266,-0.938959638045275));
#23988=CARTESIAN_POINT('Ctrl Pts',(96.8622380739791,1.39940510139645,-1.10192330390906));
#23989=CARTESIAN_POINT('Ctrl Pts',(96.8541870796653,1.31347879053693,-1.20305403662124));
#23990=CARTESIAN_POINT('Ctrl Pts',(96.8439816841957,1.19823149971852,-1.31147941733016));
#23991=CARTESIAN_POINT('Ctrl Pts',(96.8422929274682,1.17895161599672,-1.32883782466348));
#23992=CARTESIAN_POINT('Ctrl Pts',(96.8396152696973,1.14811150398895,-1.35540476904008));
#23993=CARTESIAN_POINT('Ctrl Pts',(96.8386383424385,1.13680424710619,-1.36490226579022));
#23994=CARTESIAN_POINT('Ctrl Pts',(96.8368092764201,1.11554103092052,-1.38231472511466));
#23995=CARTESIAN_POINT('Ctrl Pts',(96.8359586845422,1.10561587078853,-1.39026591797298));
#23996=CARTESIAN_POINT('Ctrl Pts',(96.8340489897373,1.08325654407973,-1.40778744865554));
#23997=CARTESIAN_POINT('Ctrl Pts',(96.8329877187508,1.07077935444391,-1.41730088103467));
#23998=CARTESIAN_POINT('Ctrl Pts',(96.8297841041277,1.03297298845034,-1.44534275452274));
#23999=CARTESIAN_POINT('Ctrl Pts',(96.8276226358796,1.00727834127237,-1.46336564074575));
#24000=CARTESIAN_POINT('Ctrl Pts',(96.8185664509998,0.898917599066307,-1.53516627141331));
#24001=CARTESIAN_POINT('Ctrl Pts',(96.811455655941,0.81233261622961,-1.58268724357425));
#24002=CARTESIAN_POINT('Ctrl Pts',(96.7959342835873,0.618097373257478,-1.66913755217854));
#24003=CARTESIAN_POINT('Ctrl Pts',(96.787527262531,0.509700516808075,-1.70536615208122));
#24004=CARTESIAN_POINT('Ctrl Pts',(96.7783701481369,0.382235149323251,-1.73471652008209));
#24005=CARTESIAN_POINT('Ctrl Pts',(96.7772064725435,0.365844861631656,-1.7382470200084));
#24006=CARTESIAN_POINT('Ctrl Pts',(96.7754547019485,0.340841890758904,-1.74326336792976));
#24007=CARTESIAN_POINT('Ctrl Pts',(96.7748579231204,0.332264672024242,-1.74491849675535));
#24008=CARTESIAN_POINT('Ctrl Pts',(96.7738258132042,0.317320833625288,-1.74768799218558));
#24009=CARTESIAN_POINT('Ctrl Pts',(96.7733889280089,0.310960023286738,-1.74883095138706));
#24010=CARTESIAN_POINT('Ctrl Pts',(96.7723529463956,0.295793426421174,-1.75147083497368));
#24011=CARTESIAN_POINT('Ctrl Pts',(96.7717556252265,0.286982412952275,-1.75293609127932));
#24012=CARTESIAN_POINT('Ctrl Pts',(96.7699447204414,0.260081762698165,-1.75720135335226));
#24013=CARTESIAN_POINT('Ctrl Pts',(96.7687422729645,0.24195894002122,-1.75978835517912));
#24014=CARTESIAN_POINT('Ctrl Pts',(96.7625597454069,0.147636856093194,-1.77176792695457));
#24015=CARTESIAN_POINT('Ctrl Pts',(96.7577851106945,0.0709192489455892,
-1.7764941094718));
#24016=CARTESIAN_POINT('Ctrl Pts',(96.7441089652802,-0.151044211140708,
-1.77576046135922));
#24017=CARTESIAN_POINT('Ctrl Pts',(96.735325674491,-0.29559556672042,-1.757486540941));
#24018=CARTESIAN_POINT('Ctrl Pts',(96.7243516674893,-0.46018271977652,-1.71578043049605));
#24019=CARTESIAN_POINT('Ctrl Pts',(96.7227455294568,-0.483927164842429,
-1.70923521602991));
#24020=CARTESIAN_POINT('Ctrl Pts',(96.7201786996517,-0.52127452056922,-1.69809974207909));
#24021=CARTESIAN_POINT('Ctrl Pts',(96.7192285837694,-0.534971580149367,
-1.69383448067292));
#24022=CARTESIAN_POINT('Ctrl Pts',(96.7174224905945,-0.560758845091712,
-1.6854603528706));
#24023=CARTESIAN_POINT('Ctrl Pts',(96.7165677019335,-0.572859391300981,
-1.68138609085725));
#24024=CARTESIAN_POINT('Ctrl Pts',(96.7146110089703,-0.600315581739159,
-1.67181078479785));
#24025=CARTESIAN_POINT('Ctrl Pts',(96.7135064496511,-0.615641290931902,
-1.66622803593303));
#24026=CARTESIAN_POINT('Ctrl Pts',(96.7100235335237,-0.663411453859677,
-1.64807761402416));
#24027=CARTESIAN_POINT('Ctrl Pts',(96.7076207609489,-0.695563154064766,
-1.63476792936696));
#24028=CARTESIAN_POINT('Ctrl Pts',(96.6937390335091,-0.876686123266674,
-1.55347876953772));
#24029=CARTESIAN_POINT('Ctrl Pts',(96.6815930563486,-1.01606866320442,-1.46610413578739));
#24030=CARTESIAN_POINT('Ctrl Pts',(96.6661110590931,-1.18011048251419,-1.32851252615373));
#24031=CARTESIAN_POINT('Ctrl Pts',(96.6625100550054,-1.21734797909129,-1.29447717529465));
#24032=CARTESIAN_POINT('Ctrl Pts',(96.6580900043349,-1.26241103564533,-1.24962210628938));
#24033=CARTESIAN_POINT('Ctrl Pts',(96.6571823650173,-1.27162924224538,-1.2402403507054));
#24034=CARTESIAN_POINT('Ctrl Pts',(96.6557437545782,-1.28619605233158,-1.22508192362801));
#24035=CARTESIAN_POINT('Ctrl Pts',(96.6552079220928,-1.29161173312698,-1.21937079740525));
#24036=CARTESIAN_POINT('Ctrl Pts',(96.6541728136703,-1.30205756909306,-1.2082074208869));
#24037=CARTESIAN_POINT('Ctrl Pts',(96.6536732582095,-1.30709179193982,-1.20275938366372));
#24038=CARTESIAN_POINT('Ctrl Pts',(96.6524385004021,-1.31951275176329,-1.18914732869402));
#24039=CARTESIAN_POINT('Ctrl Pts',(96.651706323875,-1.32685815605473,-1.18094568906797));
#24040=CARTESIAN_POINT('Ctrl Pts',(96.6488848347251,-1.35506155260926,-1.14885932101553));
#24041=CARTESIAN_POINT('Ctrl Pts',(96.6468324401498,-1.37535607572425,-1.12448455208884));
#24042=CARTESIAN_POINT('Ctrl Pts',(96.6412985837889,-1.42904987669197,-1.05636546342158));
#24043=CARTESIAN_POINT('Ctrl Pts',(96.6378781070863,-1.46108743043736,-1.01159077213557));
#24044=CARTESIAN_POINT('Ctrl Pts',(96.625895426446,-1.56668879639517,-0.848496135349694));
#24045=CARTESIAN_POINT('Ctrl Pts',(96.6174789699763,-1.62836431512253,-0.723108821659154));
#24046=CARTESIAN_POINT('Ctrl Pts',(96.6068065877054,-1.68374202177313,-0.566395027436137));
#24047=CARTESIAN_POINT('Ctrl Pts',(96.6050595035203,-1.69214216132003,-0.540782124792592));
#24048=CARTESIAN_POINT('Ctrl Pts',(96.6022195674877,-1.70470915709253,-0.49929903048888));
#24049=CARTESIAN_POINT('Ctrl Pts',(96.6011386633855,-1.70924474836109,-0.483544405806046));
#24050=CARTESIAN_POINT('Ctrl Pts',(96.5992026814816,-1.71692595921063,-0.455403734900474));
#24051=CARTESIAN_POINT('Ctrl Pts',(96.5983504495468,-1.72015725176205,-0.443042126367992));
#24052=CARTESIAN_POINT('Ctrl Pts',(96.5965353242905,-1.72672115443602,-0.4167763521796));
#24053=CARTESIAN_POINT('Ctrl Pts',(96.595571401331,-1.73001978891778,-0.402864719259183));
#24054=CARTESIAN_POINT('Ctrl Pts',(96.5929478934363,-1.7384916303543,-0.365111052016149));
#24055=CARTESIAN_POINT('Ctrl Pts',(96.5912781628921,-1.74334199502644,-0.341200548374984));
#24056=CARTESIAN_POINT('Ctrl Pts',(96.5817055613514,-1.7680890875309,-0.204849284669015));
#24057=CARTESIAN_POINT('Ctrl Pts',(96.5734788508433,-1.77759572881467,-0.0908146220477611));
#24058=CARTESIAN_POINT('Ctrl Pts',(96.5571171173897,-1.77465459210713,0.133152362411942));
#24059=CARTESIAN_POINT('Ctrl Pts',(96.5490302069568,-1.76302821151447,0.24261845888245));
#24060=CARTESIAN_POINT('Ctrl Pts',(96.5401427424422,-1.7380023145234,0.367018082674013));
#24061=CARTESIAN_POINT('Ctrl Pts',(96.5389597378287,-1.73440197901315,0.383671925961179));
#24062=CARTESIAN_POINT('Ctrl Pts',(96.5371849554004,-1.72858113267848,0.408838149382176));
#24063=CARTESIAN_POINT('Ctrl Pts',(96.5365841627788,-1.72653622047425,0.417389569006045));
#24064=CARTESIAN_POINT('Ctrl Pts',(96.5355482086114,-1.72287884313549,0.432197042775446));
#24065=CARTESIAN_POINT('Ctrl Pts',(96.5351114445457,-1.72129566806455,0.438459825230202));
#24066=CARTESIAN_POINT('Ctrl Pts',(96.5340796085663,-1.71745742429487,0.453302042837895));
#24067=CARTESIAN_POINT('Ctrl Pts',(96.5334862631617,-1.71517221410322,0.461873392487705));
#24068=CARTESIAN_POINT('Ctrl Pts',(96.5317001716538,-1.70805928496215,0.487771512037753));
#24069=CARTESIAN_POINT('Ctrl Pts',(96.5305181217489,-1.70303235320524,0.505043002069628));
#24070=CARTESIAN_POINT('Ctrl Pts',(96.5245505631103,-1.67606501526009,0.592711473787468));
#24071=CARTESIAN_POINT('Ctrl Pts',(96.519954996623,-1.65001653625175,0.661776890872312));
#24072=CARTESIAN_POINT('Ctrl Pts',(96.5068822695579,-1.56302711957404,0.85504869015209));
#24073=CARTESIAN_POINT('Ctrl Pts',(96.4985313059506,-1.4918003819241,0.974007725420844));
#24074=CARTESIAN_POINT('Ctrl Pts',(96.4877152114919,-1.38894045266001,1.10762581092684));
#24075=CARTESIAN_POINT('Ctrl Pts',(96.4857420444112,-1.36975760484689,1.13126232407069));
#24076=CARTESIAN_POINT('Ctrl Pts',(96.4827142410135,-1.33977131520348,1.1663290797827));
#24077=CARTESIAN_POINT('Ctrl Pts',(96.4816774162574,-1.32940720942422,1.17812866210799));
#24078=CARTESIAN_POINT('Ctrl Pts',(96.4797890995996,-1.31036930358091,1.19923229620853));
#24079=CARTESIAN_POINT('Ctrl Pts',(96.4789399092411,-1.30174934812967,1.20858364716928));
#24080=CARTESIAN_POINT('Ctrl Pts',(96.4770961581717,-1.28291336977222,1.22858254266602));
#24081=CARTESIAN_POINT('Ctrl Pts',(96.4761001779779,-1.27266366454852,1.23919689819363));
#24082=CARTESIAN_POINT('Ctrl Pts',(96.4732913139656,-1.24355764176133,1.26859641044473));
#24083=CARTESIAN_POINT('Ctrl Pts',(96.4714656991539,-1.2244102876338,1.28708654517838));
#24084=CARTESIAN_POINT('Ctrl Pts',(96.4633963602737,-1.13882490605257,1.366095794733));
#24085=CARTESIAN_POINT('Ctrl Pts',(96.4569667847527,-1.06827307513788,1.42194525163768));
#24086=CARTESIAN_POINT('Ctrl Pts',(96.4433371859864,-0.912941161386405,
1.52680127853941));
#24087=CARTESIAN_POINT('Ctrl Pts',(96.4361404218093,-0.827713155058399,
1.57463487062948));
#24088=CARTESIAN_POINT('Ctrl Pts',(96.4261688189721,-0.701580409632603,
1.6323422453525));
#24089=CARTESIAN_POINT('Ctrl Pts',(96.4232485465996,-0.663586414707914,
1.64815349117786));
#24090=CARTESIAN_POINT('Ctrl Pts',(96.4195336166109,-0.613482778854462,
1.66699019298297));
#24091=CARTESIAN_POINT('Ctrl Pts',(96.4186801307191,-0.601845341461083,
1.67122698344178));
#24092=CARTESIAN_POINT('Ctrl Pts',(96.417306757995,-0.582898082576699,1.67790143775753));
#24093=CARTESIAN_POINT('Ctrl Pts',(96.4167827245249,-0.575615275422439,
1.68041377938165));
#24094=CARTESIAN_POINT('Ctrl Pts',(96.4157518178152,-0.56117800374746,1.68528931496328));
#24095=CARTESIAN_POINT('Ctrl Pts',(96.4152448489529,-0.55402444100427,1.68765451138728));
#24096=CARTESIAN_POINT('Ctrl Pts',(96.4139644220206,-0.535827106669778,
1.69354295640146));
#24097=CARTESIAN_POINT('Ctrl Pts',(96.4131944978607,-0.524763260831761,
1.69700382183262));
#24098=CARTESIAN_POINT('Ctrl Pts',(96.4100038060226,-0.478445366633006,
1.71099614012119));
#24099=CARTESIAN_POINT('Ctrl Pts',(96.4076334123019,-0.442899790959773,
1.72054002336557));
#24100=CARTESIAN_POINT('Ctrl Pts',(96.4008339555867,-0.338578973672684,
1.74510198813008));
#24101=CARTESIAN_POINT('Ctrl Pts',(96.3965046475898,-0.269174501310736,
1.75714629565119));
#24102=CARTESIAN_POINT('Ctrl Pts',(96.3846705863581,-0.0776647030914143,
1.77876354208276));
#24103=CARTESIAN_POINT('Ctrl Pts',(96.3771914645592,0.044983665069589,1.77988877837057));
#24104=CARTESIAN_POINT('Ctrl Pts',(96.3677409052407,0.191008860547269,1.76611791284723));
#24105=CARTESIAN_POINT('Ctrl Pts',(96.3661583834715,0.21519832509185,1.76333390372538));
#24106=CARTESIAN_POINT('Ctrl Pts',(96.3635334544907,0.2548285964531,1.75794520631995));
#24107=CARTESIAN_POINT('Ctrl Pts',(96.3625001708429,0.270306194993132,1.75563193658893));
#24108=CARTESIAN_POINT('Ctrl Pts',(96.3606155653953,0.298300232662472,1.75106901804026));
#24109=CARTESIAN_POINT('Ctrl Pts',(96.3597665013136,0.31082704559568,1.74888886668231));
#24110=CARTESIAN_POINT('Ctrl Pts',(96.3579198721308,0.337880542826909,1.74388067319088));
#24111=CARTESIAN_POINT('Ctrl Pts',(96.3569208516996,0.352397356328795,1.74100521069526));
#24112=CARTESIAN_POINT('Ctrl Pts',(96.3540941761324,0.393127212887685,1.7324072507934));
#24113=CARTESIAN_POINT('Ctrl Pts',(96.3522535279206,0.4192480019455,1.72627195541064));
#24114=CARTESIAN_POINT('Ctrl Pts',(96.3440523731365,0.533819771847705,1.69660747711912));
#24115=CARTESIAN_POINT('Ctrl Pts',(96.3374987069675,0.620502449168482,1.66685714959223));
#24116=CARTESIAN_POINT('Ctrl Pts',(96.3235070215871,0.797011289586751,1.59059541409464));
#24117=CARTESIAN_POINT('Ctrl Pts',(96.3160705031135,0.885956855749489,1.54282270175741));
#24118=CARTESIAN_POINT('Ctrl Pts',(96.3062131562096,1.00118573274527,1.46766637619235));
#24119=CARTESIAN_POINT('Ctrl Pts',(96.3036096164551,1.03137014099969,1.44661450672097));
#24120=CARTESIAN_POINT('Ctrl Pts',(96.3002303851703,1.07046138216396,1.41750455676896));
#24121=CARTESIAN_POINT('Ctrl Pts',(96.2994078450249,1.0799697658581,1.41027375486372));
#24122=CARTESIAN_POINT('Ctrl Pts',(96.2981232201638,1.09481969916538,1.39874261022068));
#24123=CARTESIAN_POINT('Ctrl Pts',(96.2976568923052,1.10021032251459,1.39450647671594));
#24124=CARTESIAN_POINT('Ctrl Pts',(96.2966887355916,1.11140468636307,1.38560424972168));
#24125=CARTESIAN_POINT('Ctrl Pts',(96.2961873526501,1.11720382714097,1.38093270114255));
#24126=CARTESIAN_POINT('Ctrl Pts',(96.2949409812768,1.13161898218803,1.36917020583847));
#24127=CARTESIAN_POINT('Ctrl Pts',(96.2941991468169,1.14019807023773,1.36203412219907));
#24128=CARTESIAN_POINT('Ctrl Pts',(96.2912880446905,1.17383069700094,1.33351801322075));
#24129=CARTESIAN_POINT('Ctrl Pts',(96.2891587559039,1.1983564231411,1.31152239921838));
#24130=CARTESIAN_POINT('Ctrl Pts',(96.2833354685803,1.26467847131537,1.24862734835433));
#24131=CARTESIAN_POINT('Ctrl Pts',(96.2797104551052,1.3050900172544,1.20632618976675));
#24132=CARTESIAN_POINT('Ctrl Pts',(96.2673226776806,1.43669522453664,1.05419633114055));
#24133=CARTESIAN_POINT('Ctrl Pts',(96.2586804255489,1.51669502649027,0.935443912564588));
#24134=CARTESIAN_POINT('Ctrl Pts',(96.2478686974002,1.59286224310267,0.786424385262114));
#24135=CARTESIAN_POINT('Ctrl Pts',(96.2462595860244,1.60363719519756,0.764212724515875));
#24136=CARTESIAN_POINT('Ctrl Pts',(96.2436803695459,1.61999837073896,0.728614730398607));
#24137=CARTESIAN_POINT('Ctrl Pts',(96.2427207925812,1.62588978183821,0.715371611745342));
#24138=CARTESIAN_POINT('Ctrl Pts',(96.2409918423764,1.63615184356162,0.691522067783552));
#24139=CARTESIAN_POINT('Ctrl Pts',(96.2402245927433,1.64058311021227,0.680942488945931));
#24140=CARTESIAN_POINT('Ctrl Pts',(96.2384157300193,1.65074135086279,0.656015016335219));
#24141=CARTESIAN_POINT('Ctrl Pts',(96.2373713403672,1.65638414220848,0.641634051628717));
#24142=CARTESIAN_POINT('Ctrl Pts',(96.2342725213628,1.67247030227617,0.59901067821534));
#24143=CARTESIAN_POINT('Ctrl Pts',(96.2322007862062,1.68238347140754,0.570575470139431));
#24144=CARTESIAN_POINT('Ctrl Pts',(96.2273542462392,1.70363730076587,0.504230979717622));
#24145=CARTESIAN_POINT('Ctrl Pts',(96.2245640897837,1.71444323059226,0.466168368994196));
#24146=CARTESIAN_POINT('Ctrl Pts',(96.2103175552787,1.76253107758018,0.272372181807902));
#24147=CARTESIAN_POINT('Ctrl Pts',(96.1983478358472,1.77989868591278,0.112495978105697));
#24148=CARTESIAN_POINT('Ctrl Pts',(96.1869838792615,1.77561363799549,-0.047542308152177));
#24149=CARTESIAN_POINT('Ctrl Pts',(96.0403469426785,1.77561363837197,-0.0475422940912497));
#24150=CARTESIAN_POINT('Ctrl Pts',(96.0433876696981,1.77672830932013,-0.00591146882942374));
#24151=CARTESIAN_POINT('Ctrl Pts',(96.0464401059596,1.77637919693629,0.0357703223646982));
#24152=CARTESIAN_POINT('Ctrl Pts',(96.0546368358133,1.77148391667716,0.147967372245616));
#24153=CARTESIAN_POINT('Ctrl Pts',(96.0597534565257,1.7642023552637,0.218269494084479));
#24154=CARTESIAN_POINT('Ctrl Pts',(96.0659341402809,1.74990412066124,0.305300748148632));
#24155=CARTESIAN_POINT('Ctrl Pts',(96.0671549786533,1.74679738129867,0.322601837170153));
#24156=CARTESIAN_POINT('Ctrl Pts',(96.0689631289445,1.7417622012224,0.348432004388496));
#24157=CARTESIAN_POINT('Ctrl Pts',(96.0695602857837,1.74002688401859,0.356997028436484));
#24158=CARTESIAN_POINT('Ctrl Pts',(96.070588108326,1.73691281003247,0.371804810633909));
#24159=CARTESIAN_POINT('Ctrl Pts',(96.0710203752537,1.73556349610133,0.378053278305842));
#24160=CARTESIAN_POINT('Ctrl Pts',(96.0720385473342,1.7322911826648,0.392820024996573));
#24161=CARTESIAN_POINT('Ctrl Pts',(96.0726227983545,1.73033906837447,0.401331571240553));
#24162=CARTESIAN_POINT('Ctrl Pts',(96.0743707824079,1.72427664982682,0.426897929467039));
#24163=CARTESIAN_POINT('Ctrl Pts',(96.0755243800255,1.71997625030062,0.443907155502213));
#24164=CARTESIAN_POINT('Ctrl Pts',(96.0853751304822,1.68072435477487,0.590014484111818));
#24165=CARTESIAN_POINT('Ctrl Pts',(96.0934208631937,1.63154246615937,0.714864172440539));
#24166=CARTESIAN_POINT('Ctrl Pts',(96.1070040804877,1.52813008816765,0.909617282520516));
#24167=CARTESIAN_POINT('Ctrl Pts',(96.112404552365,1.4819079180233,0.983123405205661));
#24168=CARTESIAN_POINT('Ctrl Pts',(96.1196814438005,1.41503649597352,1.07397244150562));
#24169=CARTESIAN_POINT('Ctrl Pts',(96.121380762951,1.39910597314861,1.09464489762381));
#24170=CARTESIAN_POINT('Ctrl Pts',(96.1240558468793,1.37358794487497,1.1262913368892));
#24171=CARTESIAN_POINT('Ctrl Pts',(96.1250192586575,1.36431065498018,1.13751150910192));
#24172=CARTESIAN_POINT('Ctrl Pts',(96.1268265678247,1.34675290542148,1.15822246489308));
#24173=CARTESIAN_POINT('Ctrl Pts',(96.1276689986667,1.33850734416403,1.16774172742074));
#24174=CARTESIAN_POINT('Ctrl Pts',(96.1295647570431,1.31981993366253,1.18885781453425));
#24175=CARTESIAN_POINT('Ctrl Pts',(96.1306202658558,1.30932519381584,1.20040621048101));
#24176=CARTESIAN_POINT('Ctrl Pts',(96.1338209049152,1.27724161463002,1.23478960843855));
#24177=CARTESIAN_POINT('Ctrl Pts',(96.135985300139,1.25519864763659,1.25719038166149));
#24178=CARTESIAN_POINT('Ctrl Pts',(96.1477549634364,1.13355718658271,1.37441704113651));
#24179=CARTESIAN_POINT('Ctrl Pts',(96.157821035613,1.02380768668753,1.4580053342488));
#24180=CARTESIAN_POINT('Ctrl Pts',(96.1732379316871,0.842205515268603,1.56562277283818));
#24181=CARTESIAN_POINT('Ctrl Pts',(96.1785816332144,0.776587420662064,1.59918693063103));
#24182=CARTESIAN_POINT('Ctrl Pts',(96.184999997342,0.692655181488947,1.63573022676487));
#24183=CARTESIAN_POINT('Ctrl Pts',(96.1862440509095,0.676132737364651,1.64262873409602));
#24184=CARTESIAN_POINT('Ctrl Pts',(96.1880794531956,0.651335127631088,1.65254473206552));
#24185=CARTESIAN_POINT('Ctrl Pts',(96.1886810694911,0.643137810137824,1.65575218720448));
#24186=CARTESIAN_POINT('Ctrl Pts',(96.1897135534512,0.628944183604309,1.66118456939699));
#24187=CARTESIAN_POINT('Ctrl Pts',(96.1901460725971,0.622959349878934,1.66343818991849));
#24188=CARTESIAN_POINT('Ctrl Pts',(96.1911605071167,0.608830551604378,1.66867151256132));
#24189=CARTESIAN_POINT('Ctrl Pts',(96.1917408189518,0.600676784961151,1.67162396049337));
#24190=CARTESIAN_POINT('Ctrl Pts',(96.1934646049107,0.576255166025127,1.68026516813738));
#24191=CARTESIAN_POINT('Ctrl Pts',(96.1945983531944,0.559925278218729,1.68577720611461));
#24192=CARTESIAN_POINT('Ctrl Pts',(96.2045386443326,0.414666030370205,1.73246466599179));
#24193=CARTESIAN_POINT('Ctrl Pts',(96.2126743007798,0.281485631032072,1.75902191816467));
#24194=CARTESIAN_POINT('Ctrl Pts',(96.2248460825533,0.0846217228168619,
1.77532154072611));
#24195=CARTESIAN_POINT('Ctrl Pts',(96.2287060933793,0.0224549346748234,
1.77719508028112));
#24196=CARTESIAN_POINT('Ctrl Pts',(96.2344516118664,-0.0680520708919391,
1.77517278840987));
#24197=CARTESIAN_POINT('Ctrl Pts',(96.2362691830766,-0.0964049428039959,
1.7738589203888));
#24198=CARTESIAN_POINT('Ctrl Pts',(96.2396191519547,-0.148019174782241,
1.77022604542378));
#24199=CARTESIAN_POINT('Ctrl Pts',(96.2411448299046,-0.171289706317521,
1.76812603663042));
#24200=CARTESIAN_POINT('Ctrl Pts',(96.2436070434258,-0.208418346636026,
1.7640356038368));
#24201=CARTESIAN_POINT('Ctrl Pts',(96.2445343259482,-0.222306562133279,
1.76233923871774));
#24202=CARTESIAN_POINT('Ctrl Pts',(96.2463121651587,-0.248744028302583,
1.75879258206465));
#24203=CARTESIAN_POINT('Ctrl Pts',(96.2471617438501,-0.261296381246172,
1.75697157775804));
#24204=CARTESIAN_POINT('Ctrl Pts',(96.2491095719971,-0.289883074080024,
1.75251131530876));
#24205=CARTESIAN_POINT('Ctrl Pts',(96.250210481592,-0.305902653254055,1.74978617064578));
#24206=CARTESIAN_POINT('Ctrl Pts',(96.2537739408441,-0.35729954370982,1.74031551234671));
#24207=CARTESIAN_POINT('Ctrl Pts',(96.2562631869044,-0.392507867695139,
1.73271414088731));
#24208=CARTESIAN_POINT('Ctrl Pts',(96.2680562970163,-0.556012279196441,
1.69217503082626));
#24209=CARTESIAN_POINT('Ctrl Pts',(96.2777641414023,-0.680581183691712,
1.64602699985076));
#24210=CARTESIAN_POINT('Ctrl Pts',(96.2926867390598,-0.86313744528844,1.5541041965456));
#24211=CARTESIAN_POINT('Ctrl Pts',(96.2979070116048,-0.925411846684418,
1.51784748875361));
#24212=CARTESIAN_POINT('Ctrl Pts',(96.3041963347968,-1.00006800558042,1.46807434499025));
#24213=CARTESIAN_POINT('Ctrl Pts',(96.3054278745845,-1.01466997481802,1.45802030169281));
#24214=CARTESIAN_POINT('Ctrl Pts',(96.3072485941074,-1.03626610921513,1.44266887800989));
#24215=CARTESIAN_POINT('Ctrl Pts',(96.3078478126449,-1.04337504487847,1.43753590028861));
#24216=CARTESIAN_POINT('Ctrl Pts',(96.3088777837763,-1.05560161226745,1.42856927621761));
#24217=CARTESIAN_POINT('Ctrl Pts',(96.3093101608457,-1.0607368512459,1.42476042781098));
#24218=CARTESIAN_POINT('Ctrl Pts',(96.3103265740201,-1.07281431573213,1.41570097896848));
#24219=CARTESIAN_POINT('Ctrl Pts',(96.3109089796608,-1.07973864910677,1.41042698339383));
#24220=CARTESIAN_POINT('Ctrl Pts',(96.312645604051,-1.10038632688025,1.39445927286749));
#24221=CARTESIAN_POINT('Ctrl Pts',(96.3137898806864,-1.11399206816059,1.38361427421799));
#24222=CARTESIAN_POINT('Ctrl Pts',(96.3236830509232,-1.23137028798669,1.28719917402009));
#24223=CARTESIAN_POINT('Ctrl Pts',(96.3317713689111,-1.32528550275458,1.19028701106267));
#24224=CARTESIAN_POINT('Ctrl Pts',(96.3453768613518,-1.46001872358041,1.01531125352363));
#24225=CARTESIAN_POINT('Ctrl Pts',(96.3507522415374,-1.50761113602867,0.943195547056151));
#24226=CARTESIAN_POINT('Ctrl Pts',(96.3579985654031,-1.56249522315527,0.845192756360054));
#24227=CARTESIAN_POINT('Ctrl Pts',(96.3596942673656,-1.57471695663431,0.822197367381114));
#24228=CARTESIAN_POINT('Ctrl Pts',(96.3623649211322,-1.59297145358098,0.785950142298659));
#24229=CARTESIAN_POINT('Ctrl Pts',(96.363327588463,-1.59935455688939,0.772878165226385));
#24230=CARTESIAN_POINT('Ctrl Pts',(96.365134230964,-1.61096321881567,0.74834497333285));
#24231=CARTESIAN_POINT('Ctrl Pts',(96.3659767492329,-1.61622884697976,0.736903651485344));
#24232=CARTESIAN_POINT('Ctrl Pts',(96.3678736692495,-1.62775133562321,0.711149517456909));
#24233=CARTESIAN_POINT('Ctrl Pts',(96.3689302643824,-1.63394189280763,0.69680837430314));
#24234=CARTESIAN_POINT('Ctrl Pts',(96.3716628616095,-1.64936603126019,0.659740454729706));
#24235=CARTESIAN_POINT('Ctrl Pts',(96.3733480820901,-1.65831913977624,0.636901325841086));
#24236=CARTESIAN_POINT('Ctrl Pts',(96.3828308320086,-1.70559024865233,0.508552713885142));
#24237=CARTESIAN_POINT('Ctrl Pts',(96.3909356923378,-1.73430634666039,0.399797134784209));
#24238=CARTESIAN_POINT('Ctrl Pts',(96.4048153245524,-1.7652170892738,0.212397340106992));
#24239=CARTESIAN_POINT('Ctrl Pts',(96.4105192306627,-1.77281950760008,0.134966303210488));
#24240=CARTESIAN_POINT('Ctrl Pts',(96.4188796824323,-1.77657836423367,0.0184727949455617));
#24241=CARTESIAN_POINT('Ctrl Pts',(96.4216299180277,-1.77655774068567,-0.020372277207449));
#24242=CARTESIAN_POINT('Ctrl Pts',(96.4251344145167,-1.77487271739594,-0.0709118418405051));
#24243=CARTESIAN_POINT('Ctrl Pts',(96.4259418866715,-1.77436572233193,-0.0826314368179974));
#24244=CARTESIAN_POINT('Ctrl Pts',(96.4272564624798,-1.77334359385232,-0.101847955948175));
#24245=CARTESIAN_POINT('Ctrl Pts',(96.4277671680262,-1.7728969338977,-0.109347956134689));
#24246=CARTESIAN_POINT('Ctrl Pts',(96.4287250655545,-1.77196497090298,-0.123484739922586));
#24247=CARTESIAN_POINT('Ctrl Pts',(96.4291728358794,-1.77148993859981,-0.130122020595905));
#24248=CARTESIAN_POINT('Ctrl Pts',(96.4303630914379,-1.77012193802916,-0.147837422565275));
#24249=CARTESIAN_POINT('Ctrl Pts',(96.4311019554302,-1.76916226152398,-0.158910311858289));
#24250=CARTESIAN_POINT('Ctrl Pts',(96.4338576862862,-1.76516804958806,-0.200458834120121));
#24251=CARTESIAN_POINT('Ctrl Pts',(96.4358406527299,-1.76144927286057,-0.230865134721124));
#24252=CARTESIAN_POINT('Ctrl Pts',(96.4454400694956,-1.73934312049414,-0.379582379965967));
#24253=CARTESIAN_POINT('Ctrl Pts',(96.4526573165571,-1.70981173014821,-0.495929869578268));
#24254=CARTESIAN_POINT('Ctrl Pts',(96.4637288019037,-1.64833128176214,-0.664557910971128));
#24255=CARTESIAN_POINT('Ctrl Pts',(96.4674452769705,-1.62504982414338,-0.719614846062477));
#24256=CARTESIAN_POINT('Ctrl Pts',(96.4738015453543,-1.58148570479922,-0.809686700392552));
#24257=CARTESIAN_POINT('Ctrl Pts',(96.4763962804471,-1.56270156170168,-0.845371532595011));
#24258=CARTESIAN_POINT('Ctrl Pts',(96.4801534427757,-1.5342314550302,-0.895260447356261));
#24259=CARTESIAN_POINT('Ctrl Pts',(96.4812811005627,-1.52552769655476,-0.910012439086788));
#24260=CARTESIAN_POINT('Ctrl Pts',(96.4832628764201,-1.50996609696092,-0.935536987169152));
#24261=CARTESIAN_POINT('Ctrl Pts',(96.484113496306,-1.50320278989333,-0.946365905034824));
#24262=CARTESIAN_POINT('Ctrl Pts',(96.4858873889435,-1.48892937979577,-0.968680371648061));
#24263=CARTESIAN_POINT('Ctrl Pts',(96.4868112745153,-1.48140175994041,-0.980153644933));
#24264=CARTESIAN_POINT('Ctrl Pts',(96.4892349744694,-1.46141612195033,-1.00985867771676));
#24265=CARTESIAN_POINT('Ctrl Pts',(96.4907425631872,-1.44875006570373,-1.02794688618169));
#24266=CARTESIAN_POINT('Ctrl Pts',(96.49818793437,-1.38508582745041,-1.11535033611063));
#24267=CARTESIAN_POINT('Ctrl Pts',(96.5043037030689,-1.32944107081139,-1.18112303845155));
#24268=CARTESIAN_POINT('Ctrl Pts',(96.5118167459577,-1.25688101990635,-1.25523988945663));
#24269=CARTESIAN_POINT('Ctrl Pts',(96.5131024092744,-1.24431617937507,-1.26769645646042));
#24270=CARTESIAN_POINT('Ctrl Pts',(96.5221645659548,-1.15466056927883,-1.3539621794663));
#24271=CARTESIAN_POINT('Ctrl Pts',(96.530043952294,-1.07123923731331,-1.42088091225778));
#24272=CARTESIAN_POINT('Ctrl Pts',(96.5397276826587,-0.957863715944365,
-1.49613578613419));
#24273=CARTESIAN_POINT('Ctrl Pts',(96.5417919842727,-0.933014410136437,
-1.51175710276556));
#24274=CARTESIAN_POINT('Ctrl Pts',(96.5445784839781,-0.898387234334779,
-1.5323459308134));
#24275=CARTESIAN_POINT('Ctrl Pts',(96.5453301387442,-0.888934962664311,
-1.53784860176916));
#24276=CARTESIAN_POINT('Ctrl Pts',(96.5465730130397,-0.873108762295881,
-1.54686719589485));
#24277=CARTESIAN_POINT('Ctrl Pts',(96.5470672177115,-0.866763066909204,
-1.55043181908437));
#24278=CARTESIAN_POINT('Ctrl Pts',(96.5480822799548,-0.853616688444252,
-1.55771070791429));
#24279=CARTESIAN_POINT('Ctrl Pts',(96.5486028097194,-0.846813321125198,
-1.56141964419779));
#24280=CARTESIAN_POINT('Ctrl Pts',(96.5499772098976,-0.82869249927194,-1.57114514878173));
#24281=CARTESIAN_POINT('Ctrl Pts',(96.5508263816818,-0.817333581725103,
-1.57708407407204));
#24282=CARTESIAN_POINT('Ctrl Pts',(96.5551020271408,-0.759374605681323,
-1.60659306537321));
#24283=CARTESIAN_POINT('Ctrl Pts',(96.5584248076811,-0.711811154827843,
-1.62822512342973));
#24284=CARTESIAN_POINT('Ctrl Pts',(96.5714322160051,-0.519039592306961,
-1.7058328833121));
#24285=CARTESIAN_POINT('Ctrl Pts',(96.5806989043514,-0.367715596809096,
-1.74472237467166));
#24286=CARTESIAN_POINT('Ctrl Pts',(96.5930611443431,-0.174662267186891,
-1.76806910819083));
#24287=CARTESIAN_POINT('Ctrl Pts',(96.5955637586065,-0.135928738473593,
-1.77146783994708));
#24288=CARTESIAN_POINT('Ctrl Pts',(96.5991229796369,-0.0815787027146657,
-1.774443896111));
#24289=CARTESIAN_POINT('Ctrl Pts',(96.6001465887385,-0.0660303159480231,
-1.77509047577077));
#24290=CARTESIAN_POINT('Ctrl Pts',(96.6020282643681,-0.0376133813468859,
-1.77589832832862));
#24291=CARTESIAN_POINT('Ctrl Pts',(96.6028842613908,-0.0247476284584036,
-1.77612420146555));
#24292=CARTESIAN_POINT('Ctrl Pts',(96.6046319301138,0.00138780180533268,
-1.77629901797108));
#24293=CARTESIAN_POINT('Ctrl Pts',(96.605523824763,0.0146566984927439,-1.77623908633274));
#24294=CARTESIAN_POINT('Ctrl Pts',(96.6077640674554,0.0478053536630558,
-1.77571791160041));
#24295=CARTESIAN_POINT('Ctrl Pts',(96.6091181104532,0.0676799444655246,
-1.77507149782045));
#24296=CARTESIAN_POINT('Ctrl Pts',(96.6147739406371,0.150001128646456,-1.77100953250991));
#24297=CARTESIAN_POINT('Ctrl Pts',(96.6191659716135,0.212249872353845,-1.76463126019965));
#24298=CARTESIAN_POINT('Ctrl Pts',(96.6331581257644,0.405555032149858,-1.73444822129257));
#24299=CARTESIAN_POINT('Ctrl Pts',(96.6430303293577,0.534342874064152,-1.69919340268804));
#24300=CARTESIAN_POINT('Ctrl Pts',(96.655876815425,0.699883962047843,-1.63317543163726));
#24301=CARTESIAN_POINT('Ctrl Pts',(96.6590881093104,0.741142795399371,-1.61487078335525));
#24302=CARTESIAN_POINT('Ctrl Pts',(96.6631040800162,0.793064946139255,-1.58942545474513));
#24303=CARTESIAN_POINT('Ctrl Pts',(96.6639797182553,0.804406910224268,-1.58371551458119));
#24304=CARTESIAN_POINT('Ctrl Pts',(96.6653764441158,0.822547079259722,-1.57433795632047));
#24305=CARTESIAN_POINT('Ctrl Pts',(96.6659019966978,0.829384054015543,-1.57074689081819));
#24306=CARTESIAN_POINT('Ctrl Pts',(96.6669243759083,0.842710641585863,-1.56363593437802));
#24307=CARTESIAN_POINT('Ctrl Pts',(96.6674214063263,0.849202070046048,-1.56011999787408));
#24308=CARTESIAN_POINT('Ctrl Pts',(96.6686593057921,0.865395468100679,-1.55121819094696));
#24309=CARTESIAN_POINT('Ctrl Pts',(96.6693970401735,0.875069456169091,-1.54578156760805));
#24310=CARTESIAN_POINT('Ctrl Pts',(96.6723066555768,0.913283222007781,-1.52383232481876));
#24311=CARTESIAN_POINT('Ctrl Pts',(96.6744383799482,0.941413649170928,-1.50661603066987));
#24312=CARTESIAN_POINT('Ctrl Pts',(96.6802815351733,1.01827539865973,-1.45658133462302));
#24313=CARTESIAN_POINT('Ctrl Pts',(96.6839230924121,1.06588414887998,-1.42211318219492));
#24314=CARTESIAN_POINT('Ctrl Pts',(96.69631499456,1.22283334070916,-1.29616607858894));
#24315=CARTESIAN_POINT('Ctrl Pts',(96.7049467586127,1.32282044426029,-1.19394722468504));
#24316=CARTESIAN_POINT('Ctrl Pts',(96.7157432994021,1.42451295597466,-1.06133588654701));
#24317=CARTESIAN_POINT('Ctrl Pts',(96.7173492678694,1.4390958717733,-1.04147683657097));
#24318=CARTESIAN_POINT('Ctrl Pts',(96.7199187398832,1.46153734585777,-1.00954438249589));
#24319=CARTESIAN_POINT('Ctrl Pts',(96.7208717053221,1.46967050890309,-0.997667203171026));
#24320=CARTESIAN_POINT('Ctrl Pts',(96.7226618598118,1.48458956479065,-0.975301952876253));
#24321=CARTESIAN_POINT('Ctrl Pts',(96.7234976402743,1.49141095618452,-0.964838546688172));
#24322=CARTESIAN_POINT('Ctrl Pts',(96.725398302095,1.50659549054344,-0.941000999097562));
#24323=CARTESIAN_POINT('Ctrl Pts',(96.7264655730623,1.51489187641334,-0.927585805821953));
#24324=CARTESIAN_POINT('Ctrl Pts',(96.7297408577931,1.53964693316766,-0.886338992089204));
#24325=CARTESIAN_POINT('Ctrl Pts',(96.7319694919433,1.55552450219238,-0.858168266225254));
#24326=CARTESIAN_POINT('Ctrl Pts',(96.7403645968453,1.61174598138914,-0.75172569841525));
#24327=CARTESIAN_POINT('Ctrl Pts',(96.7466945303134,1.64701713193903,-0.670930299409452));
#24328=CARTESIAN_POINT('Ctrl Pts',(96.7611247440834,1.71255543260793,-0.484063713797703));
#24329=CARTESIAN_POINT('Ctrl Pts',(96.7692472197254,1.73924085386397,-0.377103476463024));
#24330=CARTESIAN_POINT('Ctrl Pts',(96.7788481038222,1.75970956422427,-0.24317732411605));
#24331=CARTESIAN_POINT('Ctrl Pts',(96.7806338299924,1.7630162474474,-0.217914742085545));
#24332=CARTESIAN_POINT('Ctrl Pts',(96.7831088341323,1.76690185795227,-0.182288854331869));
#24333=CARTESIAN_POINT('Ctrl Pts',(96.7838199674651,1.7679350852835,-0.171979502887705));
#24334=CARTESIAN_POINT('Ctrl Pts',(96.7850202134992,1.76953761293301,-0.154444852038142));
#24335=CARTESIAN_POINT('Ctrl Pts',(96.7855117906169,1.7701529981727,-0.147224138254561));
#24336=CARTESIAN_POINT('Ctrl Pts',(96.7865394568458,1.77135327007756,-0.132043011563271));
#24337=CARTESIAN_POINT('Ctrl Pts',(96.7870750331009,1.77192872025303,-0.124082153946712));
#24338=CARTESIAN_POINT('Ctrl Pts',(96.7885351515605,1.77335877469186,-0.102253395420015));
#24339=CARTESIAN_POINT('Ctrl Pts',(96.7894539095615,1.77410438136053,-0.0883785851909835));
#24340=CARTESIAN_POINT('Ctrl Pts',(96.7909547797782,1.77506420704411,-0.0655130360673177));
#24341=CARTESIAN_POINT('Ctrl Pts',(96.7915411706753,1.77537303872842,-0.0565282306894022));
#24342=CARTESIAN_POINT('Ctrl Pts',(96.7921246220486,1.77561363846711,-0.047542290537889));
#24343=CARTESIAN_POINT('Origin',(88.3562164250559,0.,0.));
#24344=CARTESIAN_POINT('',(97.6892780533294,1.77561363837197,-0.0475422940912403));
#24345=CARTESIAN_POINT('',(97.5395352881717,1.77561363837197,-0.0475422940912395));
#24346=CARTESIAN_POINT('',(88.3562164250559,1.77561363837197,-0.0475422940912398));
#24347=CARTESIAN_POINT('Ctrl Pts',(97.6892780533294,1.77561363837197,-0.0475422940912433));
#24348=CARTESIAN_POINT('Ctrl Pts',(97.6872059749121,1.77472582019844,-0.080700602655293));
#24349=CARTESIAN_POINT('Ctrl Pts',(97.6851152451758,1.77290879404315,-0.113849259557775));
#24350=CARTESIAN_POINT('Ctrl Pts',(97.6806364708754,1.7670940076383,-0.183894415182408));
#24351=CARTESIAN_POINT('Ctrl Pts',(97.6782450379417,1.76287138399518,-0.220731882255648));
#24352=CARTESIAN_POINT('Ctrl Pts',(97.6747361193426,1.75510518458071,-0.273756943199008));
#24353=CARTESIAN_POINT('Ctrl Pts',(97.6736474005101,1.75248279157628,-0.290070866414429));
#24354=CARTESIAN_POINT('Ctrl Pts',(97.6717006908093,1.74742110409714,-0.318979729331859));
#24355=CARTESIAN_POINT('Ctrl Pts',(97.6708456224853,1.74507220682892,-0.331589446336467));
#24356=CARTESIAN_POINT('Ctrl Pts',(97.669042604046,1.73985854588832,-0.357986854608185));
#24357=CARTESIAN_POINT('Ctrl Pts',(97.668093819272,1.73696598277814,-0.371768076281808));
#24358=CARTESIAN_POINT('Ctrl Pts',(97.6655566998686,1.72883910770633,-0.408320061348677));
#24359=CARTESIAN_POINT('Ctrl Pts',(97.6639593385852,1.72331900063188,-0.431023739565304));
#24360=CARTESIAN_POINT('Ctrl Pts',(97.6603949302854,1.71012270780295,-0.480984368508529));
#24361=CARTESIAN_POINT('Ctrl Pts',(97.6584217520089,1.70223942238302,-0.508179528390899));
#24362=CARTESIAN_POINT('Ctrl Pts',(97.6520898680133,1.67512629676021,-0.59398680048482));
#24363=CARTESIAN_POINT('Ctrl Pts',(97.6476633667186,1.65349353828367,-0.651786997527286));
#24364=CARTESIAN_POINT('Ctrl Pts',(97.6335112575606,1.57575405025281,-0.830556815984747));
#24365=CARTESIAN_POINT('Ctrl Pts',(97.6236126737745,1.50902138815495,-0.946404820769795));
#24366=CARTESIAN_POINT('Ctrl Pts',(97.6129231006762,1.4187223644381,-1.06894789901965));
#24367=CARTESIAN_POINT('Ctrl Pts',(97.6116053584319,1.40724356906661,-1.08401492949707));
#24368=CARTESIAN_POINT('Ctrl Pts',(97.6096801718675,1.38992531466666,-1.10600796578824));
#24369=CARTESIAN_POINT('Ctrl Pts',(97.6090611096744,1.38427077678759,-1.11307700823375));
#24370=CARTESIAN_POINT('Ctrl Pts',(97.6079582936657,1.37403887302606,-1.12566988621387));
#24371=CARTESIAN_POINT('Ctrl Pts',(97.6074731939136,1.36948182745627,-1.13120955020389));
#24372=CARTESIAN_POINT('Ctrl Pts',(97.6063863084202,1.35914454050102,-1.14362179648143));
#24373=CARTESIAN_POINT('Ctrl Pts',(97.6057858764029,1.35334560902482,-1.15047832078638));
#24374=CARTESIAN_POINT('Ctrl Pts',(97.603955411395,1.33540497343696,-1.17136755068604));
#24375=CARTESIAN_POINT('Ctrl Pts',(97.6027368675409,1.32309474437322,-1.18525471775049));
#24376=CARTESIAN_POINT('Ctrl Pts',(97.5998748291708,1.29337237119081,-1.21774423169152));
#24377=CARTESIAN_POINT('Ctrl Pts',(97.5982426183236,1.27577286867829,-1.23617022497075));
#24378=CARTESIAN_POINT('Ctrl Pts',(97.5920008791105,1.20624964612288,-1.30589134202646));
#24379=CARTESIAN_POINT('Ctrl Pts',(97.5875181803793,1.15157744389617,-1.3543490075586));
#24380=CARTESIAN_POINT('Ctrl Pts',(97.5757606191815,1.00069315986174,-1.47232075007208));
#24381=CARTESIAN_POINT('Ctrl Pts',(97.5685006649299,0.900247588891457,-1.53579477853656));
#24382=CARTESIAN_POINT('Ctrl Pts',(97.5592883796332,0.772338233827302,-1.59973653764129));
#24383=CARTESIAN_POINT('Ctrl Pts',(97.5576974749325,0.750218651166703,-1.61022831287166));
#24384=CARTESIAN_POINT('Ctrl Pts',(97.5550615636616,0.713580035458728,-1.62668795506153));
#24385=CARTESIAN_POINT('Ctrl Pts',(97.5540258162919,0.699185784466034,-1.63292663111069));
#24386=CARTESIAN_POINT('Ctrl Pts',(97.5521386309304,0.672976875088629,-1.64387588136404));
#24387=CARTESIAN_POINT('Ctrl Pts',(97.5512894811523,0.661190549053708,-1.64865182227883));
#24388=CARTESIAN_POINT('Ctrl Pts',(97.5494448649821,0.63560814548388,-1.65869962647025));
#24389=CARTESIAN_POINT('Ctrl Pts',(97.5484479682849,0.621795653474599,-1.66392677356525));
#24390=CARTESIAN_POINT('Ctrl Pts',(97.5456337397525,0.582851037159355,-1.67811220152573));
#24391=CARTESIAN_POINT('Ctrl Pts',(97.5438035982459,0.557580840590902,-1.68667701826366));
#24392=CARTESIAN_POINT('Ctrl Pts',(97.5356947627728,0.445916840385493,-1.72173967235312));
#24393=CARTESIAN_POINT('Ctrl Pts',(97.5292280445423,0.357777737364824,-1.74218831686148));
#24394=CARTESIAN_POINT('Ctrl Pts',(97.5154906050832,0.171087062149514,-1.77073429190682));
#24395=CARTESIAN_POINT('Ctrl Pts',(97.5082226129462,0.0726266187703843,
-1.77749726256714));
#24396=CARTESIAN_POINT('Ctrl Pts',(97.4982865671146,-0.0657028737945895,
-1.77548100536618));
#24397=CARTESIAN_POINT('Ctrl Pts',(97.4954623440966,-0.105491033016684,
-1.77356190921816));
#24398=CARTESIAN_POINT('Ctrl Pts',(97.4918482775702,-0.157405191377807,
-1.76930439050472));
#24399=CARTESIAN_POINT('Ctrl Pts',(97.4910033791617,-0.169615947802007,
-1.76817557724141));
#24400=CARTESIAN_POINT('Ctrl Pts',(97.4896403558562,-0.189451448365353,
-1.76613452273223));
#24401=CARTESIAN_POINT('Ctrl Pts',(97.4891181939661,-0.197083449343026,
-1.76529915973207));
#24402=CARTESIAN_POINT('Ctrl Pts',(97.4880876951923,-0.212216245105763,
-1.76354343023716));
#24403=CARTESIAN_POINT('Ctrl Pts',(97.4875792935411,-0.219717022735083,
-1.76262463370563));
#24404=CARTESIAN_POINT('Ctrl Pts',(97.4862903944107,-0.23881477204022,-1.76016147962614));
#24405=CARTESIAN_POINT('Ctrl Pts',(97.4855135265019,-0.25040300953272,-1.758550335021));
#24406=CARTESIAN_POINT('Ctrl Pts',(97.4822488346855,-0.299382631131891,
-1.75124657307073));
#24407=CARTESIAN_POINT('Ctrl Pts',(97.4798143526546,-0.336605825583204,
-1.74447456493271));
#24408=CARTESIAN_POINT('Ctrl Pts',(97.4727348916702,-0.445812056599596,
-1.72098039604626));
#24409=CARTESIAN_POINT('Ctrl Pts',(97.4681995612666,-0.517002094852825,
-1.70095038621736));
#24410=CARTESIAN_POINT('Ctrl Pts',(97.456465972274,-0.697422097458739,-1.63780859854279));
#24411=CARTESIAN_POINT('Ctrl Pts',(97.4492796176422,-0.803982434135849,
-1.58821377609273));
#24412=CARTESIAN_POINT('Ctrl Pts',(97.4401477387012,-0.925968296669926,
-1.51599725511932));
#24413=CARTESIAN_POINT('Ctrl Pts',(97.4385547338565,-0.946800645888214,
-1.5030746513076));
#24414=CARTESIAN_POINT('Ctrl Pts',(97.4359160716854,-0.980523463569613,
-1.48117663037636));
#24415=CARTESIAN_POINT('Ctrl Pts',(97.4348797076883,-0.993574523347515,
-1.47245377283426));
#24416=CARTESIAN_POINT('Ctrl Pts',(97.4329918750813,-1.01698677046804,-1.45635287971364));
#24417=CARTESIAN_POINT('Ctrl Pts',(97.4321427023145,-1.0273876826591,-1.44903427723535));
#24418=CARTESIAN_POINT('Ctrl Pts',(97.430298582419,-1.04968874435795,-1.43298132699448));
#24419=CARTESIAN_POINT('Ctrl Pts',(97.4293022111883,-1.06156032244852,-1.42420911469984));
#24420=CARTESIAN_POINT('Ctrl Pts',(97.4264910588254,-1.09454981975061,-1.39919070027944));
#24421=CARTESIAN_POINT('Ctrl Pts',(97.4246635131647,-1.11541276598836,-1.38261641498715));
#24422=CARTESIAN_POINT('Ctrl Pts',(97.416577347391,-1.20514525780377,-1.3079766182692));
#24423=CARTESIAN_POINT('Ctrl Pts',(97.4101319519,-1.26990434962579,-1.24519742111886));
#24424=CARTESIAN_POINT('Ctrl Pts',(97.3964564160723,-1.39458129060194,-1.10444835506477));
#24425=CARTESIAN_POINT('Ctrl Pts',(97.3892293069433,-1.45336672559103,-1.02585997100196));
#24426=CARTESIAN_POINT('Ctrl Pts',(97.3792729241883,-1.52690890717147,-0.908437954332116));
#24427=CARTESIAN_POINT('Ctrl Pts',(97.3763936824957,-1.54726285173968,-0.873320421127474));
#24428=CARTESIAN_POINT('Ctrl Pts',(97.3727217778804,-1.57221259036916,-0.826658166702527));
#24429=CARTESIAN_POINT('Ctrl Pts',(97.37187191239,-1.57791438770333,-0.815721987251617));
#24430=CARTESIAN_POINT('Ctrl Pts',(97.3705029029085,-1.58698712218242,-0.797869107188291));
#24431=CARTESIAN_POINT('Ctrl Pts',(97.3699796586266,-1.5904277268772,-0.790988552047881));
#24432=CARTESIAN_POINT('Ctrl Pts',(97.368948933866,-1.59715352074858,-0.777316922696418));
#24433=CARTESIAN_POINT('Ctrl Pts',(97.3684413707099,-1.60044034370457,-0.770526883092213));
#24434=CARTESIAN_POINT('Ctrl Pts',(97.3671574189369,-1.60868708293115,-0.753210023192963));
#24435=CARTESIAN_POINT('Ctrl Pts',(97.3663846039688,-1.61358710124694,-0.742654801724874));
#24436=CARTESIAN_POINT('Ctrl Pts',(97.3631633602325,-1.63372155593118,-0.698142567250437));
#24437=CARTESIAN_POINT('Ctrl Pts',(97.360766519699,-1.64799166739871,-0.663756793432768));
#24438=CARTESIAN_POINT('Ctrl Pts',(97.3538526883113,-1.686595543225,-0.561796150403388));
#24439=CARTESIAN_POINT('Ctrl Pts',(97.3494394367805,-1.70792610792445,-0.49316249557375));
#24440=CARTESIAN_POINT('Ctrl Pts',(97.3376486367997,-1.75370725297439,-0.306647598850043));
#24441=CARTESIAN_POINT('Ctrl Pts',(97.3302904810495,-1.77043637693051,-0.187277883783365));
#24442=CARTESIAN_POINT('Ctrl Pts',(97.3209711507413,-1.77590400877838,-0.0427287498799004));
#24443=CARTESIAN_POINT('Ctrl Pts',(97.3193835348976,-1.77632365132989,-0.0183026660531491));
#24444=CARTESIAN_POINT('Ctrl Pts',(97.3167519319475,-1.77618541557409,0.0217959979527274));
#24445=CARTESIAN_POINT('Ctrl Pts',(97.3157171507233,-1.77592395982576,0.03746676737239));
#24446=CARTESIAN_POINT('Ctrl Pts',(97.3138309782691,-1.77507480664552,0.0658422154165484));
#24447=CARTESIAN_POINT('Ctrl Pts',(97.3129818632966,-1.77455795980832,0.0785480701765516));
#24448=CARTESIAN_POINT('Ctrl Pts',(97.3111364635747,-1.77314548069506,0.106007639902053));
#24449=CARTESIAN_POINT('Ctrl Pts',(97.310138738753,-1.77220203153463,0.120757822955018));
#24450=CARTESIAN_POINT('Ctrl Pts',(97.3073196593275,-1.76903501638525,0.162154598168923));
#24451=CARTESIAN_POINT('Ctrl Pts',(97.3054854237162,-1.76639376137816,0.188764263306146));
#24452=CARTESIAN_POINT('Ctrl Pts',(97.2973407224382,-1.75214545687766,0.305446082672367));
#24453=CARTESIAN_POINT('Ctrl Pts',(97.2908402468761,-1.73424281787076,0.394599184517063));
#24454=CARTESIAN_POINT('Ctrl Pts',(97.2770047110806,-1.68263807558025,0.577643171424734));
#24455=CARTESIAN_POINT('Ctrl Pts',(97.2696719100604,-1.64768724992194,0.670872396629719));
#24456=CARTESIAN_POINT('Ctrl Pts',(97.2597675593518,-1.58857683900526,0.795600517175361));
#24457=CARTESIAN_POINT('Ctrl Pts',(97.2570298003482,-1.57089613344093,0.829965294096662));
#24458=CARTESIAN_POINT('Ctrl Pts',(97.2535070094585,-1.54620057919384,0.874342827559403));
#24459=CARTESIAN_POINT('Ctrl Pts',(97.2526702215721,-1.54018500197428,0.884896486325083));
#24460=CARTESIAN_POINT('Ctrl Pts',(97.2513169723814,-1.53020391956021,0.901996999300388));
#24461=CARTESIAN_POINT('Ctrl Pts',(97.2507965767226,-1.52630365180364,0.90858119632006));
#24462=CARTESIAN_POINT('Ctrl Pts',(97.2497663855819,-1.51845612724343,0.921635769876499));
#24463=CARTESIAN_POINT('Ctrl Pts',(97.2492565549594,-1.5145097787729,0.928106479612119));
#24464=CARTESIAN_POINT('Ctrl Pts',(97.2479592888655,-1.50431117307256,0.944590550038746));
#24465=CARTESIAN_POINT('Ctrl Pts',(97.2471755779381,-1.49800016638621,0.954567406163399));
#24466=CARTESIAN_POINT('Ctrl Pts',(97.2438358350591,-1.47048517816666,0.9971199113172));
#24467=CARTESIAN_POINT('Ctrl Pts',(97.2413362485873,-1.44831297389702,1.0290601595754));
#24468=CARTESIAN_POINT('Ctrl Pts',(97.2339619328085,-1.37878588131345,1.12251330870453));
#24469=CARTESIAN_POINT('Ctrl Pts',(97.2292077771675,-1.32842920507166,1.18167850176388));
#24470=CARTESIAN_POINT('Ctrl Pts',(97.2175659236551,-1.19630020488104,1.31775821212839));
#24471=CARTESIAN_POINT('Ctrl Pts',(97.2106811198566,-1.11081606362786,1.39057718012086));
#24472=CARTESIAN_POINT('Ctrl Pts',(97.2018789256366,-0.998881716832708,
1.46898113449752));
#24473=CARTESIAN_POINT('Ctrl Pts',(97.2002791064077,-0.978424934848719,
1.48268500023095));
#24474=CARTESIAN_POINT('Ctrl Pts',(97.1976315196005,-0.944443945374345,
1.50443912808453));
#24475=CARTESIAN_POINT('Ctrl Pts',(97.1965931564276,-0.931085496684032,
1.51274294821485));
#24476=CARTESIAN_POINT('Ctrl Pts',(97.1947032211352,-0.906728151337016,
1.52743900287166));
#24477=CARTESIAN_POINT('Ctrl Pts',(97.1938539695854,-0.895767402797125,
1.53389262777006));
#24478=CARTESIAN_POINT('Ctrl Pts',(97.1920114379733,-0.871960020407261,
1.5475680775706));
#24479=CARTESIAN_POINT('Ctrl Pts',(97.1910167537556,-0.859091006703501,
1.55474880648389));
#24480=CARTESIAN_POINT('Ctrl Pts',(97.1882154683958,-0.822812517113445,
1.57440375694013));
#24481=CARTESIAN_POINT('Ctrl Pts',(97.1863962470377,-0.799211634499652,
1.58651450011723));
#24482=CARTESIAN_POINT('Ctrl Pts',(97.1783824117319,-0.695124533531911,
1.6370146566962));
#24483=CARTESIAN_POINT('Ctrl Pts',(97.1720049753289,-0.612094162819844,
1.66983583021668));
#24484=CARTESIAN_POINT('Ctrl Pts',(97.1585270858967,-0.43506842514852,1.72483011750404));
#24485=CARTESIAN_POINT('Ctrl Pts',(97.1514306723062,-0.341007551365627,
1.74586297560811));
#24486=CARTESIAN_POINT('Ctrl Pts',(97.1414082978119,-0.203113291364408,
1.7651228170062));
#24487=CARTESIAN_POINT('Ctrl Pts',(97.1383514679536,-0.160314922159936,
1.76952348048217));
#24488=CARTESIAN_POINT('Ctrl Pts',(97.1344939003206,-0.104873976243193,
1.77319569920614));
#24489=CARTESIAN_POINT('Ctrl Pts',(97.1336287794512,-0.0923435747748574,
1.77389239396708));
#24490=CARTESIAN_POINT('Ctrl Pts',(97.1322413848747,-0.0720747270036096,
1.77480398802844));
#24491=CARTESIAN_POINT('Ctrl Pts',(97.1317148143736,-0.0643406747606824,
1.77510119305181));
#24492=CARTESIAN_POINT('Ctrl Pts',(97.1306832296948,-0.0491027974133395,
1.77558703367662));
#24493=CARTESIAN_POINT('Ctrl Pts',(97.1301780788872,-0.0415993020025549,
1.77577867441447));
#24494=CARTESIAN_POINT('Ctrl Pts',(97.1289085389308,-0.0226430246713958,
1.77614260265007));
#24495=CARTESIAN_POINT('Ctrl Pts',(97.1281475614745,-0.0111891226172256,
1.77625169170191));
#24496=CARTESIAN_POINT('Ctrl Pts',(97.1250492133195,0.0357787533883522,
1.7762446737839));
#24497=CARTESIAN_POINT('Ctrl Pts',(97.1227586406784,0.0712867991049795,
1.7751743152286));
#24498=CARTESIAN_POINT('Ctrl Pts',(97.1162950305329,0.172845117764904,1.76906024427386));
#24499=CARTESIAN_POINT('Ctrl Pts',(97.1122105058241,0.238679117805502,1.76138668741203));
#24500=CARTESIAN_POINT('Ctrl Pts',(97.1002246383258,0.430868106740661,1.72800891534555));
#24501=CARTESIAN_POINT('Ctrl Pts',(97.0923726650692,0.55501253424185,1.69222314860588));
#24502=CARTESIAN_POINT('Ctrl Pts',(97.0823745223659,0.698493225962655,1.63335890088485));
#24503=CARTESIAN_POINT('Ctrl Pts',(97.0806650065087,0.722570553588963,1.62285112223711));
#24504=CARTESIAN_POINT('Ctrl Pts',(97.0779617095857,0.759868485290847,1.60557904907658));
#24505=CARTESIAN_POINT('Ctrl Pts',(97.0769802924953,0.773252909511442,1.59917607325386));
#24506=CARTESIAN_POINT('Ctrl Pts',(97.0751471079851,0.797953545575903,1.58697694172729));
#24507=CARTESIAN_POINT('Ctrl Pts',(97.0742969456289,0.809290845786817,1.58122546997481));
#24508=CARTESIAN_POINT('Ctrl Pts',(97.0723937785026,0.834402295125258,1.56814549233746));
#24509=CARTESIAN_POINT('Ctrl Pts',(97.0713386752196,0.848143445752201,1.56075627294693));
#24510=CARTESIAN_POINT('Ctrl Pts',(97.0681735957177,0.888816656263697,1.53818876349456));
#24511=CARTESIAN_POINT('Ctrl Pts',(97.0660451740991,0.915450476266847,1.52248807480269));
#24512=CARTESIAN_POINT('Ctrl Pts',(97.0610386058693,0.976415652249444,1.48437081837268));
#24513=CARTESIAN_POINT('Ctrl Pts',(97.0581436265264,1.01040655970784,1.46144531268299));
#24514=CARTESIAN_POINT('Ctrl Pts',(97.049258427071,1.11102903602351,1.38839029939366));
#24515=CARTESIAN_POINT('Ctrl Pts',(97.0431680248593,1.17494992942416,1.33472986932186));
#24516=CARTESIAN_POINT('Ctrl Pts',(97.0307192152893,1.29730785162441,1.21638951963325));
#24517=CARTESIAN_POINT('Ctrl Pts',(97.0243771319298,1.35524452362216,1.15148867475972));
#24518=CARTESIAN_POINT('Ctrl Pts',(97.0169997496471,1.4193385354125,1.0681179724614));
#24519=CARTESIAN_POINT('Ctrl Pts',(97.0157295545419,1.43025070804374,1.05346137012385));
#24520=CARTESIAN_POINT('Ctrl Pts',(97.0138599260109,1.44615416754452,1.03139800501371));
#24521=CARTESIAN_POINT('Ctrl Pts',(97.0132497800798,1.45131853483857,1.02411827448091));
#24522=CARTESIAN_POINT('Ctrl Pts',(97.012155890293,1.46053464249223,1.01091744804623));
#24523=CARTESIAN_POINT('Ctrl Pts',(97.0116709082636,1.46460559487596,1.00501044000254));
#24524=CARTESIAN_POINT('Ctrl Pts',(97.0105756303623,1.47376438546499,0.991547060228764));
#24525=CARTESIAN_POINT('Ctrl Pts',(97.0099667970941,1.47883001295977,0.983976035451259));
#24526=CARTESIAN_POINT('Ctrl Pts',(97.0080828446287,1.49441571386986,0.960289589506029));
#24527=CARTESIAN_POINT('Ctrl Pts',(97.0068202079099,1.5047326768303,0.944041347951515));
#24528=CARTESIAN_POINT('Ctrl Pts',(97.0038335954327,1.52875814735824,0.904808589507813));
#24529=CARTESIAN_POINT('Ctrl Pts',(97.0021222800539,1.54221559549797,0.88167526036637));
#24530=CARTESIAN_POINT('Ctrl Pts',(96.9953707256256,1.59377530975649,0.78824875730905));
#24531=CARTESIAN_POINT('Ctrl Pts',(96.9904792453346,1.62763744376648,0.715719130817615));
#24532=CARTESIAN_POINT('Ctrl Pts',(96.978889146187,1.69579252162487,0.539631291163661));
#24533=CARTESIAN_POINT('Ctrl Pts',(96.9721904887946,1.72566616018116,0.434726319353921));
#24534=CARTESIAN_POINT('Ctrl Pts',(96.9635918250881,1.75030149880858,0.303508253355444));
#24535=CARTESIAN_POINT('Ctrl Pts',(96.9619890049453,1.75434757062463,0.279172174149227));
#24536=CARTESIAN_POINT('Ctrl Pts',(96.9593374885332,1.76014328628504,0.23918089587824));
#24537=CARTESIAN_POINT('Ctrl Pts',(96.9582982457689,1.76219389142332,0.223572251439364));
#24538=CARTESIAN_POINT('Ctrl Pts',(96.9564073833407,1.76552582789372,0.19530596532271));
#24539=CARTESIAN_POINT('Ctrl Pts',(96.9555580951217,1.76687916796851,0.182657768429895));
#24540=CARTESIAN_POINT('Ctrl Pts',(96.9537162525086,1.76950588575419,0.155337834371209));
#24541=CARTESIAN_POINT('Ctrl Pts',(96.9527223026571,1.77073287188001,0.140662703501392));
#24542=CARTESIAN_POINT('Ctrl Pts',(96.9499253081035,1.77365474898305,0.0995677215331412));
#24543=CARTESIAN_POINT('Ctrl Pts',(96.9481097057095,1.77494160268787,0.0731236978369465));
#24544=CARTESIAN_POINT('Ctrl Pts',(96.944100004836,1.77646235425336,0.0152542663560143));
#24545=CARTESIAN_POINT('Ctrl Pts',(96.941899944293,1.77645395205389,-0.0161581873154769));
#24546=CARTESIAN_POINT('Ctrl Pts',(96.9396785576437,1.77561363837197,-0.0475422940912364));
#24547=CARTESIAN_POINT('Ctrl Pts',(96.7921246220486,1.77561363846711,-0.047542290537889));
#24548=CARTESIAN_POINT('Ctrl Pts',(96.7964447788134,1.77739515555032,0.0189939657997468));
#24549=CARTESIAN_POINT('Ctrl Pts',(96.8006048204907,1.77543573913087,0.0855923702015854));
#24550=CARTESIAN_POINT('Ctrl Pts',(96.812453165962,1.75903281059313,0.276651251963474));
#24551=CARTESIAN_POINT('Ctrl Pts',(96.8200135814896,1.73517407008014,0.399877807502835));
#24552=CARTESIAN_POINT('Ctrl Pts',(96.8306304720267,1.68616500917452,0.560095940657845));
#24553=CARTESIAN_POINT('Ctrl Pts',(96.8333516475131,1.67232381214624,0.600160416610597));
#24554=CARTESIAN_POINT('Ctrl Pts',(96.8372865232963,1.65062767335898,0.656362528423919));
#24555=CARTESIAN_POINT('Ctrl Pts',(96.8384618042765,1.64394012962833,0.67293706732107));
#24556=CARTESIAN_POINT('Ctrl Pts',(96.8404906809162,1.6320511108791,0.701167645391426));
#24557=CARTESIAN_POINT('Ctrl Pts',(96.8413400898277,1.62697192878429,0.712873918648169));
#24558=CARTESIAN_POINT('Ctrl Pts',(96.8430925787236,1.61628800597513,0.736788696637372));
#24559=CARTESIAN_POINT('Ctrl Pts',(96.8439960697155,1.61067002940363,0.748990347658202));
#24560=CARTESIAN_POINT('Ctrl Pts',(96.8463034153427,1.59604883355745,0.779820645789451));
#24561=CARTESIAN_POINT('Ctrl Pts',(96.8477137014826,1.58685773829916,0.798357422382559));
#24562=CARTESIAN_POINT('Ctrl Pts',(96.8540677960926,1.54433598719296,0.880479525270836));
#24563=CARTESIAN_POINT('Ctrl Pts',(96.8591329785776,1.50749654764157,0.942162202374973));
#24564=CARTESIAN_POINT('Ctrl Pts',(96.8695931636956,1.42548878223303,1.06229706485265));
#24565=CARTESIAN_POINT('Ctrl Pts',(96.8749834812004,1.38020197212018,1.12050645596623));
#24566=CARTESIAN_POINT('Ctrl Pts',(96.8865198422848,1.27577202841406,1.2387660736924));
#24567=CARTESIAN_POINT('Ctrl Pts',(96.8926515950852,1.21569810877325,1.29777362695381));
#24568=CARTESIAN_POINT('Ctrl Pts',(96.8998280586781,1.13780835196938,1.36410682875712));
#24569=CARTESIAN_POINT('Ctrl Pts',(96.9010931926984,1.12377132544589,1.3756937735119));
#24570=CARTESIAN_POINT('Ctrl Pts',(96.9029532923447,1.1026399741394,1.3925974415513));
#24571=CARTESIAN_POINT('Ctrl Pts',(96.9035589159462,1.09568043352037,1.39807973407652));
#24572=CARTESIAN_POINT('Ctrl Pts',(96.9046433439711,1.08306969366155,1.40786168167976));
#24573=CARTESIAN_POINT('Ctrl Pts',(96.9051233836791,1.07743345136915,1.4121797471655));
#24574=CARTESIAN_POINT('Ctrl Pts',(96.9062050355867,1.06461167078221,1.421881379454));
#24575=CARTESIAN_POINT('Ctrl Pts',(96.9068052458399,1.05741104328753,1.42724439428766));
#24576=CARTESIAN_POINT('Ctrl Pts',(96.9086533129944,1.03498551854855,1.44368400586207));
#24577=CARTESIAN_POINT('Ctrl Pts',(96.909889252023,1.01962440202222,1.45457371095675));
#24578=CARTESIAN_POINT('Ctrl Pts',(96.9128043924381,0.982610088426438,1.47993908084542));
#24579=CARTESIAN_POINT('Ctrl Pts',(96.9144716581201,0.960805583072234,1.49418708381056));
#24580=CARTESIAN_POINT('Ctrl Pts',(96.920953376074,0.873932328040859,1.54826539454819));
#24581=CARTESIAN_POINT('Ctrl Pts',(96.925630371973,0.806635854375908,1.58436851892709));
#24582=CARTESIAN_POINT('Ctrl Pts',(96.9373240046006,0.633304977635761,1.66344073482572));
#24583=CARTESIAN_POINT('Ctrl Pts',(96.9443349296379,0.525069159632757,1.70070835108507));
#24584=CARTESIAN_POINT('Ctrl Pts',(96.9532696817117,0.390193324115174,1.73303580662048));
#24585=CARTESIAN_POINT('Ctrl Pts',(96.9548613558169,0.366261030807749,1.73825104666723));
#24586=CARTESIAN_POINT('Ctrl Pts',(96.9574928765716,0.326912764294527,1.74597701949301));
#24587=CARTESIAN_POINT('Ctrl Pts',(96.95852338655,0.311557519845261,1.74878231747823));
#24588=CARTESIAN_POINT('Ctrl Pts',(96.9603970325971,0.283749893352351,1.75348472249315));
#24589=CARTESIAN_POINT('Ctrl Pts',(96.9612378650935,0.27131039042699,1.75545245791126));
#24590=CARTESIAN_POINT('Ctrl Pts',(96.9630596054171,0.244451534714864,1.75940881024588));
#24591=CARTESIAN_POINT('Ctrl Pts',(96.9640418626066,0.230026644514653,1.76135278556069));
#24592=CARTESIAN_POINT('Ctrl Pts',(96.966799889143,0.189693454588111,1.76628439955327));
#24593=CARTESIAN_POINT('Ctrl Pts',(96.9685878122483,0.163741755030993,1.76887893836206));
#24594=CARTESIAN_POINT('Ctrl Pts',(96.9763883743647,0.0514064580066014,
1.77761655614586));
#24595=CARTESIAN_POINT('Ctrl Pts',(96.982573116723,-0.035293795279772,1.77800836838871));
#24596=CARTESIAN_POINT('Ctrl Pts',(96.9985934246228,-0.255340920855718,
1.76290052340124));
#24597=CARTESIAN_POINT('Ctrl Pts',(97.0085448120822,-0.387550199956913,
1.73862725078292));
#24598=CARTESIAN_POINT('Ctrl Pts',(97.0191600894515,-0.532520608749415,
1.69463626370219));
#24599=CARTESIAN_POINT('Ctrl Pts',(97.0203754351104,-0.549190095965706,
1.68930771652308));
#24600=CARTESIAN_POINT('Ctrl Pts',(97.0221771293506,-0.57404809235193,1.68095477367118));
#24601=CARTESIAN_POINT('Ctrl Pts',(97.0227732239686,-0.582296947066406,
1.67811514413915));
#24602=CARTESIAN_POINT('Ctrl Pts',(97.0237999986401,-0.596553967283767,
1.67308944619742));
#24603=CARTESIAN_POINT('Ctrl Pts',(97.0242322674264,-0.602571579418622,
1.67093160418261));
#24604=CARTESIAN_POINT('Ctrl Pts',(97.0252514473587,-0.616795775604597,
1.66574414372838));
#24605=CARTESIAN_POINT('Ctrl Pts',(97.0258366921472,-0.624991787644568,
1.66268633681345));
#24606=CARTESIAN_POINT('Ctrl Pts',(97.0275908110972,-0.649628707404103,
1.65328675975727));
#24607=CARTESIAN_POINT('Ctrl Pts',(97.0287494446904,-0.665998711690172,
1.64676055976514));
#24608=CARTESIAN_POINT('Ctrl Pts',(97.0345202515308,-0.747839619869079,
1.6127130873036));
#24609=CARTESIAN_POINT('Ctrl Pts',(97.0389555749711,-0.811722108132453,
1.58152363764978));
#24610=CARTESIAN_POINT('Ctrl Pts',(97.0513395237855,-0.986347753285769,
1.48288855856811));
#24611=CARTESIAN_POINT('Ctrl Pts',(97.0591630340525,-1.09181179150756,1.40704864269163));
#24612=CARTESIAN_POINT('Ctrl Pts',(97.0698164253239,-1.21629494828761,1.29504056451034));
#24613=CARTESIAN_POINT('Ctrl Pts',(97.072260109002,-1.24367609972905,1.26876826021332));
#24614=CARTESIAN_POINT('Ctrl Pts',(97.0757548194568,-1.28103053732408,1.23055481926915));
#24615=CARTESIAN_POINT('Ctrl Pts',(97.0767746761328,-1.29172150084308,1.21932765897184));
#24616=CARTESIAN_POINT('Ctrl Pts',(97.0786516633516,-1.31100480635862,1.19853897021191));
#24617=CARTESIAN_POINT('Ctrl Pts',(97.0795067625237,-1.31964300433458,1.18902127470431));
#24618=CARTESIAN_POINT('Ctrl Pts',(97.0812549079677,-1.33700048530506,1.16947439184729));
#24619=CARTESIAN_POINT('Ctrl Pts',(97.0821482008997,-1.3457120103945,1.15943944183592));
#24620=CARTESIAN_POINT('Ctrl Pts',(97.0843965969524,-1.3672393828856,1.13407223300584));
#24621=CARTESIAN_POINT('Ctrl Pts',(97.0857574831402,-1.37991034479923,1.11862001730415));
#24622=CARTESIAN_POINT('Ctrl Pts',(97.0914914487322,-1.43178841421404,1.05313180080035));
#24623=CARTESIAN_POINT('Ctrl Pts',(97.0959579958422,-1.4685516512384,1.00122875218225));
#24624=CARTESIAN_POINT('Ctrl Pts',(97.1104778902586,-1.57677748651851,0.829610029613119));
#24625=CARTESIAN_POINT('Ctrl Pts',(97.1208335988343,-1.63696940836888,0.70342456580508));
#24626=CARTESIAN_POINT('Ctrl Pts',(97.1336208900391,-1.69429936580948,0.534718315285902));
#24627=CARTESIAN_POINT('Ctrl Pts',(97.13637485676,-1.70559240627777,0.497522928713749));
#24628=CARTESIAN_POINT('Ctrl Pts',(97.1399096889589,-1.71878972359002,0.448299338157641));
#24629=CARTESIAN_POINT('Ctrl Pts',(97.1407430485851,-1.72180317668285,0.43658246831632));
#24630=CARTESIAN_POINT('Ctrl Pts',(97.142088816883,-1.72651266650006,0.417463432082526));
#24631=CARTESIAN_POINT('Ctrl Pts',(97.1426051472756,-1.72828130547131,0.410079796341151));
#24632=CARTESIAN_POINT('Ctrl Pts',(97.1436248591873,-1.73169894858246,0.395397021229398));
#24633=CARTESIAN_POINT('Ctrl Pts',(97.1441282981559,-1.73334927295381,0.388098383428364));
#24634=CARTESIAN_POINT('Ctrl Pts',(97.1454048150938,-1.73743737471039,0.369472165279576));
#24635=CARTESIAN_POINT('Ctrl Pts',(97.1461743304743,-1.7398105796098,0.358130530412814));
#24636=CARTESIAN_POINT('Ctrl Pts',(97.1494052162996,-1.74937621171833,0.310075008072325));
#24637=CARTESIAN_POINT('Ctrl Pts',(97.1518143351096,-1.75551932797031,0.273159269936031));
#24638=CARTESIAN_POINT('Ctrl Pts',(97.1587955145102,-1.77015237298934,0.164035246997141));
#24639=CARTESIAN_POINT('Ctrl Pts',(97.1632609839627,-1.77538230794254,0.0914662706970687));
#24640=CARTESIAN_POINT('Ctrl Pts',(97.1750475747397,-1.77741189813986,-0.100518833926835));
#24641=CARTESIAN_POINT('Ctrl Pts',(97.1823522785257,-1.76665170757841,-0.219624527224935));
#24642=CARTESIAN_POINT('Ctrl Pts',(97.1916080995304,-1.73941698698552,-0.360675059840408));
#24643=CARTESIAN_POINT('Ctrl Pts',(97.1931920252482,-1.73430511803478,-0.384504380974449));
#24644=CARTESIAN_POINT('Ctrl Pts',(97.1958133984703,-1.72512569111611,-0.423376840570269));
#24645=CARTESIAN_POINT('Ctrl Pts',(97.1968416349678,-1.72134746753916,-0.438485426767537));
#24646=CARTESIAN_POINT('Ctrl Pts',(97.1987128806093,-1.71415599149307,-0.46571649676011));
#24647=CARTESIAN_POINT('Ctrl Pts',(97.1995536139837,-1.71081152139738,-0.47785619461491));
#24648=CARTESIAN_POINT('Ctrl Pts',(97.2013771146071,-1.70331603933357,-0.503975365254594));
#24649=CARTESIAN_POINT('Ctrl Pts',(97.2023612533175,-1.69912140310034,-0.517941245732923));
#24650=CARTESIAN_POINT('Ctrl Pts',(97.2051302485903,-1.68690724117204,-0.556861766518304));
#24651=CARTESIAN_POINT('Ctrl Pts',(97.2069274165484,-1.67850689142334,-0.581691976034354));
#24652=CARTESIAN_POINT('Ctrl Pts',(97.2148067121049,-1.63966350286731,-0.688649913801664));
#24653=CARTESIAN_POINT('Ctrl Pts',(97.2210651056521,-1.60372282088699,-0.76863793066768));
#24654=CARTESIAN_POINT('Ctrl Pts',(97.2370371008279,-1.49907257137219,-0.961944159257952));
#24655=CARTESIAN_POINT('Ctrl Pts',(97.2468546196268,-1.42331572932107,-1.07085487533517));
#24656=CARTESIAN_POINT('Ctrl Pts',(97.257376592498,-1.32442397590784,-1.18375796618308));
#24657=CARTESIAN_POINT('Ctrl Pts',(97.2586151093142,-1.31247760969416,-1.19698971390143));
#24658=CARTESIAN_POINT('Ctrl Pts',(97.2604440171926,-1.29434748833199,-1.21647271009461));
#24659=CARTESIAN_POINT('Ctrl Pts',(97.2610445743363,-1.28831363990794,-1.22286109122872));
#24660=CARTESIAN_POINT('Ctrl Pts',(97.2621240053079,-1.27731783872516,-1.23433125113996));
#24661=CARTESIAN_POINT('Ctrl Pts',(97.2626040534628,-1.27237259472514,-1.23942828873989));
#24662=CARTESIAN_POINT('Ctrl Pts',(97.2636908072777,-1.26105210343334,-1.25095709592858));
#24663=CARTESIAN_POINT('Ctrl Pts',(97.2642960468508,-1.25465809460004,-1.25736992885211));
#24664=CARTESIAN_POINT('Ctrl Pts',(97.2661763810441,-1.23452415238336,-1.2772566269728));
#24665=CARTESIAN_POINT('Ctrl Pts',(97.2674389524133,-1.2206136181369,-1.29055679571444));
#24666=CARTESIAN_POINT('Ctrl Pts',(97.2704296508956,-1.18680397253319,-1.32184711531286));
#24667=CARTESIAN_POINT('Ctrl Pts',(97.2721449911464,-1.16670776540666,-1.33961808275311));
#24668=CARTESIAN_POINT('Ctrl Pts',(97.2789432514273,-1.08462189308028,-1.40895714980607));
#24669=CARTESIAN_POINT('Ctrl Pts',(97.283874780039,-1.01955282429897,-1.45673561465998));
#24670=CARTESIAN_POINT('Ctrl Pts',(97.2954711895805,-0.860026200855641,
-1.55792901095098));
#24671=CARTESIAN_POINT('Ctrl Pts',(97.3021365298245,-0.763492444096923,
-1.6074400867708));
#24672=CARTESIAN_POINT('Ctrl Pts',(97.3106933950468,-0.640248316684155,
-1.65703067764064));
#24673=CARTESIAN_POINT('Ctrl Pts',(97.3122910454977,-0.617251624051435,
-1.66573374581545));
#24674=CARTESIAN_POINT('Ctrl Pts',(97.3149303912862,-0.579346533057907,
-1.67918615956426));
#24675=CARTESIAN_POINT('Ctrl Pts',(97.3159626525256,-0.564542491003731,
-1.68422098122485));
#24676=CARTESIAN_POINT('Ctrl Pts',(97.3178381530711,-0.537696704700965,
-1.69295746327319));
#24677=CARTESIAN_POINT('Ctrl Pts',(97.3186790673972,-0.525678266957292,
-1.69672775196515));
#24678=CARTESIAN_POINT('Ctrl Pts',(97.3204994785212,-0.49970721178704,-1.70457268039935));
#24679=CARTESIAN_POINT('Ctrl Pts',(97.3214803078673,-0.485742726433725,
-1.70860448965804));
#24680=CARTESIAN_POINT('Ctrl Pts',(97.3242300216845,-0.446684123924979,
-1.71936392022173));
#24681=CARTESIAN_POINT('Ctrl Pts',(97.3260109410571,-0.421490431045736,
-1.72571280599883));
#24682=CARTESIAN_POINT('Ctrl Pts',(97.3337522880547,-0.312474011707557,
-1.75065569791172));
#24683=CARTESIAN_POINT('Ctrl Pts',(97.3398817255156,-0.22751398002855,-1.76370888235658));
#24684=CARTESIAN_POINT('Ctrl Pts',(97.3559399967528,-0.00706829237110624,
-1.78138294563386));
#24685=CARTESIAN_POINT('Ctrl Pts',(97.3659939781483,0.128613232912918,-1.77674882383763));
#24686=CARTESIAN_POINT('Ctrl Pts',(97.3766799138629,0.279507850834532,-1.75420542811582));
#24687=CARTESIAN_POINT('Ctrl Pts',(97.3778769871444,0.296522648170575,-1.75140963144019));
#24688=CARTESIAN_POINT('Ctrl Pts',(97.3796571816436,0.322031709003508,-1.74683567134944));
#24689=CARTESIAN_POINT('Ctrl Pts',(97.3802497230266,0.33055751129651,-1.74524239691463));
#24690=CARTESIAN_POINT('Ctrl Pts',(97.3812730700376,0.345348963089256,-1.74236593535558));
#24691=CARTESIAN_POINT('Ctrl Pts',(97.3817054220512,0.35161967246017,-1.7411113026109));
#24692=CARTESIAN_POINT('Ctrl Pts',(97.3827281659052,0.366503789168647,-1.73804962048148));
#24693=CARTESIAN_POINT('Ctrl Pts',(97.3833168496211,0.375110709306221,-1.73621239331826));
#24694=CARTESIAN_POINT('Ctrl Pts',(97.3850922947925,0.401175619673715,-1.73044571994207));
#24695=CARTESIAN_POINT('Ctrl Pts',(97.3862684459935,0.418588808355007,-1.72631623326657));
#24696=CARTESIAN_POINT('Ctrl Pts',(97.3922185767068,0.507231746150265,-1.70387460894952));
#24697=CARTESIAN_POINT('Ctrl Pts',(97.3968032529147,0.577344520500685,-1.68141262582316));
#24698=CARTESIAN_POINT('Ctrl Pts',(97.4098068981207,0.773718353630419,-1.60476158921119));
#24699=CARTESIAN_POINT('Ctrl Pts',(97.4180998167281,0.895342774546599,-1.54021384451901));
#24700=CARTESIAN_POINT('Ctrl Pts',(97.4289225824041,1.0343752584647,-1.44434531561639));
#24701=CARTESIAN_POINT('Ctrl Pts',(97.4309729684634,1.05994234757812,-1.42568846128217));
#24702=CARTESIAN_POINT('Ctrl Pts',(97.4340760512741,1.09738413411021,-1.39680239221828));
#24703=CARTESIAN_POINT('Ctrl Pts',(97.435108919311,1.10964483692882,-1.38708225078516));
#24704=CARTESIAN_POINT('Ctrl Pts',(97.4369850635182,1.1315418230313,-1.36924644871359));
#24705=CARTESIAN_POINT('Ctrl Pts',(97.4378260072926,1.14122330737616,-1.36118774723576));
#24706=CARTESIAN_POINT('Ctrl Pts',(97.4396459632077,1.1618842645315,-1.34361455493872));
#24707=CARTESIAN_POINT('Ctrl Pts',(97.4406263021129,1.17283429100162,-1.33406702244634));
#24708=CARTESIAN_POINT('Ctrl Pts',(97.4433731628355,1.20301071179697,-1.30709695413706));
#24709=CARTESIAN_POINT('Ctrl Pts',(97.4451516788816,1.22197364284283,-1.28938648683015));
#24710=CARTESIAN_POINT('Ctrl Pts',(97.4528727909988,1.30180750181456,-1.21148222811849));
#24711=CARTESIAN_POINT('Ctrl Pts',(97.4589833470828,1.35866333791957,-1.14735442500851));
#24712=CARTESIAN_POINT('Ctrl Pts',(97.4750549189262,1.49317811195947,-0.971554783332337));
#24713=CARTESIAN_POINT('Ctrl Pts',(97.4851443442598,1.56305236894657,-0.854616541608144));
#24714=CARTESIAN_POINT('Ctrl Pts',(97.4958545248844,1.62598022212548,-0.715224813145737));
#24715=CARTESIAN_POINT('Ctrl Pts',(97.4970451875861,1.63281069967429,-0.699490878835642));
#24716=CARTESIAN_POINT('Ctrl Pts',(97.4988178309789,1.64274381488037,-0.675671320992764));
#24717=CARTESIAN_POINT('Ctrl Pts',(97.4994091186317,1.64601677287129,-0.667658420661842));
#24718=CARTESIAN_POINT('Ctrl Pts',(97.5004312664794,1.65160629733246,-0.653683110942573));
#24719=CARTESIAN_POINT('Ctrl Pts',(97.5008636580802,1.65394935300564,-0.647731820814894));
#24720=CARTESIAN_POINT('Ctrl Pts',(97.5018877044466,1.65944693011367,-0.633543791320473));
#24721=CARTESIAN_POINT('Ctrl Pts',(97.5024776359595,1.66257231444965,-0.625296055382906));
#24722=CARTESIAN_POINT('Ctrl Pts',(97.5042608568555,1.67188687115351,-0.600151759963838));
#24723=CARTESIAN_POINT('Ctrl Pts',(97.5054433995845,1.67788106119412,-0.583183547937348));
#24724=CARTESIAN_POINT('Ctrl Pts',(97.5114601514787,1.70735618660297,-0.495526776001437));
#24725=CARTESIAN_POINT('Ctrl Pts',(97.5161003219243,1.72663425252144,-0.42349563145663));
#24726=CARTESIAN_POINT('Ctrl Pts',(97.5269767928662,1.76143472299729,-0.250582050110423));
#24727=CARTESIAN_POINT('Ctrl Pts',(97.5331561149429,1.77289076556361,-0.149236379042087));
#24728=CARTESIAN_POINT('Ctrl Pts',(97.5395352881717,1.77561363837197,-0.0475422940912269));
#24729=CARTESIAN_POINT('Origin',(88.3562164250559,0.,0.));
#24730=CARTESIAN_POINT('',(98.4367443001643,1.7756136383719,-0.0475422940939716));
#24731=CARTESIAN_POINT('',(98.289313862947,1.77561363837197,-0.0475422940912461));
#24732=CARTESIAN_POINT('',(88.3562164250559,1.77561363837197,-0.0475422940912398));
#24733=CARTESIAN_POINT('Ctrl Pts',(98.4367443001643,1.77561363837182,-0.0475422940967033));
#24734=CARTESIAN_POINT('Ctrl Pts',(98.4365226374283,1.77552297576021,-0.0509283690169651));
#24735=CARTESIAN_POINT('Ctrl Pts',(98.4363014139303,1.77542262597964,-0.0543142353769213));
#24736=CARTESIAN_POINT('Ctrl Pts',(98.4286423307297,1.7716056866418,-0.171754060191483));
#24737=CARTESIAN_POINT('Ctrl Pts',(98.4216940556708,1.75691583374141,-0.28520175953313));
#24738=CARTESIAN_POINT('Ctrl Pts',(98.4079341841336,1.70689092790807,-0.503668546124907));
#24739=CARTESIAN_POINT('Ctrl Pts',(98.401151729996,1.67244459277732,-0.608345121057067));
#24740=CARTESIAN_POINT('Ctrl Pts',(98.3924543515143,1.61872191312569,-0.731716303873464));
#24741=CARTESIAN_POINT('Ctrl Pts',(98.3908498136962,1.60843200433929,-0.754066159180973));
#24742=CARTESIAN_POINT('Ctrl Pts',(98.3882849468019,1.59141509328202,-0.789092966644753));
#24743=CARTESIAN_POINT('Ctrl Pts',(98.3873351652438,1.58499274876237,-0.801915004951576));
#24744=CARTESIAN_POINT('Ctrl Pts',(98.3855293391019,1.57255970802052,-0.826004280537739));
#24745=CARTESIAN_POINT('Ctrl Pts',(98.3846744785475,1.5665813571433,-0.837287252671703));
#24746=CARTESIAN_POINT('Ctrl Pts',(98.3827171014043,1.55268629428937,-0.862841618770187));
#24747=CARTESIAN_POINT('Ctrl Pts',(98.3816119228124,1.54469359885245,-0.877070146655087));
#24748=CARTESIAN_POINT('Ctrl Pts',(98.3786807758117,1.52311668573725,-0.914271198507795));
#24749=CARTESIAN_POINT('Ctrl Pts',(98.3768433345683,1.50920926710067,-0.937050434558558));
#24750=CARTESIAN_POINT('Ctrl Pts',(98.3652794628307,1.41936610879395,-1.07701513562128));
#24751=CARTESIAN_POINT('Ctrl Pts',(98.3550641054095,1.33035544637778,-1.18520161856188));
#24752=CARTESIAN_POINT('Ctrl Pts',(98.3394501219947,1.1760901985898,-1.33318366193406));
#24753=CARTESIAN_POINT('Ctrl Pts',(98.3340642890454,1.11938805249025,-1.38113696148111));
#24754=CARTESIAN_POINT('Ctrl Pts',(98.3275965216838,1.04537659153359,-1.43616748804243));
#24755=CARTESIAN_POINT('Ctrl Pts',(98.3263431814397,1.03074126028944,-1.44670722292181));
#24756=CARTESIAN_POINT('Ctrl Pts',(98.3244933039316,1.00866356401447,-1.46210147495414));
#24757=CARTESIAN_POINT('Ctrl Pts',(98.3238863674541,1.00134168787206,-1.46712567323955));
#24758=CARTESIAN_POINT('Ctrl Pts',(98.3228442049251,0.988628256098838,-1.47570998774132));
#24759=CARTESIAN_POINT('Ctrl Pts',(98.3224073046791,0.983254637283262,-1.47929581848026));
#24760=CARTESIAN_POINT('Ctrl Pts',(98.3213810435232,0.970528645119562,-1.48768792460388));
#24761=CARTESIAN_POINT('Ctrl Pts',(98.3207933377285,0.963160043479178,-1.49246907868839));
#24762=CARTESIAN_POINT('Ctrl Pts',(98.3190783443929,0.941430787727218,-1.50634025874099));
#24763=CARTESIAN_POINT('Ctrl Pts',(98.317960326134,0.926974335617681,-1.5152793591475));
#24764=CARTESIAN_POINT('Ctrl Pts',(98.3096365204388,0.817359668665095,-1.58090324273059));
#24765=CARTESIAN_POINT('Ctrl Pts',(98.3028801393751,0.717201749197308,-1.62879100508618));
#24766=CARTESIAN_POINT('Ctrl Pts',(98.2898535083788,0.518035788211802,-1.70205456398339));
#24767=CARTESIAN_POINT('Ctrl Pts',(98.2836121332032,0.420033608408203,-1.72884926171801));
#24768=CARTESIAN_POINT('Ctrl Pts',(98.2750979641418,0.289384626960589,-1.75279992892654));
#24769=CARTESIAN_POINT('Ctrl Pts',(98.2730621396235,0.258339959894389,-1.75764368547648));
#24770=CARTESIAN_POINT('Ctrl Pts',(98.269970593612,0.211616922047383,-1.76366910864739));
#24771=CARTESIAN_POINT('Ctrl Pts',(98.2689342835042,0.196023722010649,-1.76547022645596));
#24772=CARTESIAN_POINT('Ctrl Pts',(98.2670465068762,0.167757246598624,-1.76835610293289));
#24773=CARTESIAN_POINT('Ctrl Pts',(98.2661973355244,0.15509217009072,-1.7695118549669));
#24774=CARTESIAN_POINT('Ctrl Pts',(98.2643531703054,0.127702105482516,-1.77171502668333));
#24775=CARTESIAN_POINT('Ctrl Pts',(98.2633567517855,0.112974377992038,-1.77271507312335));
#24776=CARTESIAN_POINT('Ctrl Pts',(98.2605948383426,0.0723586769443952,
-1.7749647853012));
#24777=CARTESIAN_POINT('Ctrl Pts',(98.2588175748128,0.0464540697977625,
-1.77583154129507));
#24778=CARTESIAN_POINT('Ctrl Pts',(98.2478448323583,-0.112002047341471,
-1.77766408290553));
#24779=CARTESIAN_POINT('Ctrl Pts',(98.238205264741,-0.244277910121359,-1.76435544837809));
#24780=CARTESIAN_POINT('Ctrl Pts',(98.223832924817,-0.436403834762349,-1.72299579622583));
#24781=CARTESIAN_POINT('Ctrl Pts',(98.2191578161576,-0.498220721826873,
-1.70614764806835));
#24782=CARTESIAN_POINT('Ctrl Pts',(98.21209137115,-0.592034120180635,-1.67504363813668));
#24783=CARTESIAN_POINT('Ctrl Pts',(98.2096333631561,-0.624746110059658,
-1.66312003979795));
#24784=CARTESIAN_POINT('Ctrl Pts',(98.206435404249,-0.667657169603206,-1.64603382752091));
#24785=CARTESIAN_POINT('Ctrl Pts',(98.2056529700315,-0.678185084900449,
-1.64172423543386));
#24786=CARTESIAN_POINT('Ctrl Pts',(98.2043650002294,-0.695575021505212,
-1.63440984659287));
#24787=CARTESIAN_POINT('Ctrl Pts',(98.2038561949455,-0.702460609193973,
-1.63146230633669));
#24788=CARTESIAN_POINT('Ctrl Pts',(98.2028256784177,-0.716442723950815,
-1.62537199317396));
#24789=CARTESIAN_POINT('Ctrl Pts',(98.202304159467,-0.723537654254827,-1.62222611296702));
#24790=CARTESIAN_POINT('Ctrl Pts',(98.2009398865599,-0.742139755598212,
-1.61383165132288));
#24791=CARTESIAN_POINT('Ctrl Pts',(98.2001016361212,-0.75361212478544,-1.60850638910493));
#24792=CARTESIAN_POINT('Ctrl Pts',(98.1963668658106,-0.804860294422662,
-1.58404924868774));
#24793=CARTESIAN_POINT('Ctrl Pts',(98.1935428635928,-0.843974861475339,
-1.5635598011405));
#24794=CARTESIAN_POINT('Ctrl Pts',(98.1847558318783,-0.965095747324518,
-1.4942413430828));
#24795=CARTESIAN_POINT('Ctrl Pts',(98.1789641534986,-1.0439542722814,-1.44025294342655));
#24796=CARTESIAN_POINT('Ctrl Pts',(98.1676266807647,-1.18705611781828,-1.32432540184134));
#24797=CARTESIAN_POINT('Ctrl Pts',(98.1621075802911,-1.25172333746431,-1.26337885229478));
#24798=CARTESIAN_POINT('Ctrl Pts',(98.1546796392565,-1.3294126995913,-1.17831514815713));
#24799=CARTESIAN_POINT('Ctrl Pts',(98.1529566238408,-1.34682338263695,-1.15837445215766));
#24800=CARTESIAN_POINT('Ctrl Pts',(98.1502465623942,-1.37321598920205,-1.12674697635486));
#24801=CARTESIAN_POINT('Ctrl Pts',(98.1492722548657,-1.38250946637842,-1.11532437216522));
#24802=CARTESIAN_POINT('Ctrl Pts',(98.147445560409,-1.39956424930796,-1.09382164108728));
#24803=CARTESIAN_POINT('Ctrl Pts',(98.1465946862198,-1.40736140904762,-1.083771064498));
#24804=CARTESIAN_POINT('Ctrl Pts',(98.1446810272647,-1.42456575191729,-1.06109581886622));
#24805=CARTESIAN_POINT('Ctrl Pts',(98.1436160324964,-1.43391428335433,-1.0484282133084));
#24806=CARTESIAN_POINT('Ctrl Pts',(98.1408651139608,-1.45747773056723,-1.01559412229908));
#24807=CARTESIAN_POINT('Ctrl Pts',(98.1391698945206,-1.47144267951145,-0.995253279818638));
#24808=CARTESIAN_POINT('Ctrl Pts',(98.1299299124651,-1.54455691133181,-0.883853881162364));
#24809=CARTESIAN_POINT('Ctrl Pts',(98.1220999265996,-1.59567665629541,-0.787821499273327));
#24810=CARTESIAN_POINT('Ctrl Pts',(98.1083156442436,-1.66874288259566,-0.613830041084897));
#24811=CARTESIAN_POINT('Ctrl Pts',(98.1024276197712,-1.69474280435508,-0.537901312946196));
#24812=CARTESIAN_POINT('Ctrl Pts',(98.0947504353423,-1.72247193898184,-0.434594604369087));
#24813=CARTESIAN_POINT('Ctrl Pts',(98.0928436333156,-1.72883222985613,-0.408560062187443));
#24814=CARTESIAN_POINT('Ctrl Pts',(98.0896073294105,-1.73874857958756,-0.363577448623549));
#24815=CARTESIAN_POINT('Ctrl Pts',(98.0882664394465,-1.74258972100933,-0.344697438010488));
#24816=CARTESIAN_POINT('Ctrl Pts',(98.0863142891777,-1.74779435486674,-0.316799615883821));
#24817=CARTESIAN_POINT('Ctrl Pts',(98.0856909587469,-1.74939667284509,-0.307828513503592));
#24818=CARTESIAN_POINT('Ctrl Pts',(98.0845837905023,-1.75213691597315,-0.291773468410792));
#24819=CARTESIAN_POINT('Ctrl Pts',(98.0840985555096,-1.75330104728428,-0.284694523845136));
#24820=CARTESIAN_POINT('Ctrl Pts',(98.0830153387652,-1.7558166922319,-0.268796210864844));
#24821=CARTESIAN_POINT('Ctrl Pts',(98.0824186616965,-1.75714468546585,-0.25997350361966));
#24822=CARTESIAN_POINT('Ctrl Pts',(98.0806117904877,-1.76098691092547,-0.233071504715948));
#24823=CARTESIAN_POINT('Ctrl Pts',(98.0794126603786,-1.76328908890409,-0.21496250692346));
#24824=CARTESIAN_POINT('Ctrl Pts',(98.0728680335193,-1.77444059774624,-0.114942937855293));
#24825=CARTESIAN_POINT('Ctrl Pts',(98.0677612371266,-1.77786302348111,-0.0325196174557306));
#24826=CARTESIAN_POINT('Ctrl Pts',(98.0542092851574,-1.77168138552039,0.187649300816255));
#24827=CARTESIAN_POINT('Ctrl Pts',(98.0458418052931,-1.7517860784445,0.324513006834991));
#24828=CARTESIAN_POINT('Ctrl Pts',(98.0353107137848,-1.70974651376196,0.482153117889082));
#24829=CARTESIAN_POINT('Ctrl Pts',(98.03366182822,-1.7027024226322,0.506467300088243));
#24830=CARTESIAN_POINT('Ctrl Pts',(98.0310334389136,-1.69077085320271,0.544584281928687));
#24831=CARTESIAN_POINT('Ctrl Pts',(98.0300651751099,-1.6862279912027,0.558491950076518));
#24832=CARTESIAN_POINT('Ctrl Pts',(98.0282438568472,-1.67741244524881,0.584391630116195));
#24833=CARTESIAN_POINT('Ctrl Pts',(98.0273922357488,-1.67318161729964,0.596396973323348));
#24834=CARTESIAN_POINT('Ctrl Pts',(98.0254689627225,-1.66338615754936,0.62326757727564));
#24835=CARTESIAN_POINT('Ctrl Pts',(98.0243949998835,-1.65775062836051,0.638105639848719));
#24836=CARTESIAN_POINT('Ctrl Pts',(98.0211111458412,-1.6400238472746,0.682958923629991));
#24837=CARTESIAN_POINT('Ctrl Pts',(98.0188806765523,-1.6273111628562,0.712719616732592));
#24838=CARTESIAN_POINT('Ctrl Pts',(98.0106019595959,-1.57771725409396,0.820565890651796));
#24839=CARTESIAN_POINT('Ctrl Pts',(98.0043977721695,-1.53597321104229,0.896271650262331));
#24840=CARTESIAN_POINT('Ctrl Pts',(97.9903054138692,-1.43047117226747,1.05843984856373));
#24841=CARTESIAN_POINT('Ctrl Pts',(97.9823954532755,-1.36403934787121,1.14277769929264));
#24842=CARTESIAN_POINT('Ctrl Pts',(97.9727294385042,-1.27064827168052,1.24150877886826));
#24843=CARTESIAN_POINT('Ctrl Pts',(97.970707315795,-1.25038037092677,1.26191926518674));
#24844=CARTESIAN_POINT('Ctrl Pts',(97.9679625986899,-1.22174048663087,1.28939272494242));
#24845=CARTESIAN_POINT('Ctrl Pts',(97.9672118533408,-1.21378668231616,1.29688292490814));
#24846=CARTESIAN_POINT('Ctrl Pts',(97.9659665193693,-1.20038287707994,1.30927411740428));
#24847=CARTESIAN_POINT('Ctrl Pts',(97.9654689886107,-1.19497082297416,1.31421554776976));
#24848=CARTESIAN_POINT('Ctrl Pts',(97.964442223177,-1.18368010785411,1.32439702272067));
#24849=CARTESIAN_POINT('Ctrl Pts',(97.9639133722064,-1.17779694215291,1.32963169360216));
#24850=CARTESIAN_POINT('Ctrl Pts',(97.9625073710163,-1.16198092568197,1.3435169799523));
#24851=CARTESIAN_POINT('Ctrl Pts',(97.9616352344026,-1.15198612211205,1.35209672251745));
#24852=CARTESIAN_POINT('Ctrl Pts',(97.9570487077875,-1.09850509111268,1.39698234556685));
#24853=CARTESIAN_POINT('Ctrl Pts',(97.9534564902755,-1.05339165488499,1.43130726617521));
#24854=CARTESIAN_POINT('Ctrl Pts',(97.945185801493,-0.944185678737328,1.50643180065365));
#24855=CARTESIAN_POINT('Ctrl Pts',(97.9405591773055,-0.878966951924941,
1.54539356479032));
#24856=CARTESIAN_POINT('Ctrl Pts',(97.929629373244,-0.720839677627748,1.62660098704003));
#24857=CARTESIAN_POINT('Ctrl Pts',(97.9233069362445,-0.62640163384933,1.66525010040541));
#24858=CARTESIAN_POINT('Ctrl Pts',(97.9152413107957,-0.507617572906279,
1.70232154741751));
#24859=CARTESIAN_POINT('Ctrl Pts',(97.9137649937122,-0.485930335010842,
1.70863860579432));
#24860=CARTESIAN_POINT('Ctrl Pts',(97.9113573006744,-0.450694205457453,
1.71817709357557));
#24861=CARTESIAN_POINT('Ctrl Pts',(97.9104343016002,-0.437217148970669,
1.72165587087046));
#24862=CARTESIAN_POINT('Ctrl Pts',(97.9086474557629,-0.411195807127017,
1.72804741926426));
#24863=CARTESIAN_POINT('Ctrl Pts',(97.9077844044879,-0.398657958101282,
1.73098286887631));
#24864=CARTESIAN_POINT('Ctrl Pts',(97.9057602392808,-0.369330770826302,
1.73751363433028));
#24865=CARTESIAN_POINT('Ctrl Pts',(97.9045957904995,-0.352519266985833,
1.74100229120531));
#24866=CARTESIAN_POINT('Ctrl Pts',(97.9006964974025,-0.296439978558571,
1.7517941097598));
#24867=CARTESIAN_POINT('Ctrl Pts',(97.8979281115964,-0.256979177285258,
1.75801607637832));
#24868=CARTESIAN_POINT('Ctrl Pts',(97.8909912461611,-0.159013821258514,
1.77009403424395));
#24869=CARTESIAN_POINT('Ctrl Pts',(97.8867815991976,-0.100367001062135,
1.77438542427143));
#24870=CARTESIAN_POINT('Ctrl Pts',(97.8742659603391,0.0722684173030461,
1.7784316221213));
#24871=CARTESIAN_POINT('Ctrl Pts',(97.8658356941724,0.186146864378722,1.77013868261274));
#24872=CARTESIAN_POINT('Ctrl Pts',(97.8550772581095,0.334221250188591,1.74490035263605));
#24873=CARTESIAN_POINT('Ctrl Pts',(97.8525099053,0.369803807893793,1.73770729657601));
#24874=CARTESIAN_POINT('Ctrl Pts',(97.8491695754232,0.416718218583295,1.7267169172412));
#24875=CARTESIAN_POINT('Ctrl Pts',(97.8483510348131,0.428265698665458,1.72388917762427));
#24876=CARTESIAN_POINT('Ctrl Pts',(97.8470711401953,0.446415923645576,1.71925092291531));
#24877=CARTESIAN_POINT('Ctrl Pts',(97.846605593857,0.453037831890558,1.71751787173543));
#24878=CARTESIAN_POINT('Ctrl Pts',(97.8456375832112,0.466852080647597,1.71381702485344));
#24879=CARTESIAN_POINT('Ctrl Pts',(97.8451355773905,0.474042319213878,1.71184214878116));
#24880=CARTESIAN_POINT('Ctrl Pts',(97.8438853100209,0.492009119869962,1.70678549142416));
#24881=CARTESIAN_POINT('Ctrl Pts',(97.843140245577,0.502769587967576,1.70364680770171));
#24882=CARTESIAN_POINT('Ctrl Pts',(97.8401984756198,0.545431741698417,1.6907634082199));
#24883=CARTESIAN_POINT('Ctrl Pts',(97.838042826499,0.577087995457027,1.680222148401));
#24884=CARTESIAN_POINT('Ctrl Pts',(97.8321180859629,0.66449869191991,1.64835282213077));
#24885=CARTESIAN_POINT('Ctrl Pts',(97.8284209059208,0.719504709059385,1.62509676327981));
#24886=CARTESIAN_POINT('Ctrl Pts',(97.8161060884032,0.899612536774803,1.5380070647654));
#24887=CARTESIAN_POINT('Ctrl Pts',(97.807595170684,1.01828400274892,1.46214299419755));
#24888=CARTESIAN_POINT('Ctrl Pts',(97.7969174290843,1.14610632363562,1.35725053249853));
#24889=CARTESIAN_POINT('Ctrl Pts',(97.7952887999147,1.16508921265166,1.34099058125209));
#24890=CARTESIAN_POINT('Ctrl Pts',(97.7926854511532,1.1945785945918,1.31463229641913));
#24891=CARTESIAN_POINT('Ctrl Pts',(97.791721606471,1.20531517550429,1.3047955394964));
#24892=CARTESIAN_POINT('Ctrl Pts',(97.7899122073739,1.22512541035748,1.28619241744018));
#24893=CARTESIAN_POINT('Ctrl Pts',(97.789068107955,1.23422900830743,1.27745917612038));
#24894=CARTESIAN_POINT('Ctrl Pts',(97.7871498418919,1.25460151602236,1.25749441867292));
#24895=CARTESIAN_POINT('Ctrl Pts',(97.7860732558245,1.26581396448494,1.24620710780207));
#24896=CARTESIAN_POINT('Ctrl Pts',(97.7827726543576,1.29950883591614,1.2113633433446));
#24897=CARTESIAN_POINT('Ctrl Pts',(97.7805277507915,1.32149536371475,1.18733909448381));
#24898=CARTESIAN_POINT('Ctrl Pts',(97.7720276424793,1.40125802460095,1.09522281927296));
#24899=CARTESIAN_POINT('Ctrl Pts',(97.7656040654292,1.45452714375907,1.02341780103985));
#24900=CARTESIAN_POINT('Ctrl Pts',(97.7508671869894,1.56241181947067,0.852453555950466));
#24901=CARTESIAN_POINT('Ctrl Pts',(97.7425304549368,1.61342038204608,0.751455225819273));
#24902=CARTESIAN_POINT('Ctrl Pts',(97.7330012546246,1.6625408141901,0.62570806089402));
#24903=CARTESIAN_POINT('Ctrl Pts',(97.731456761187,1.6701980292724,0.604972056208978));
#24904=CARTESIAN_POINT('Ctrl Pts',(97.7293152066599,1.68040887706859,0.57564757016288));
#24905=CARTESIAN_POINT('Ctrl Pts',(97.7287014301601,1.68328732009332,0.567175392340083));
#24906=CARTESIAN_POINT('Ctrl Pts',(97.7275950720059,1.68839041301477,0.551774252266665));
#24907=CARTESIAN_POINT('Ctrl Pts',(97.7271012790119,1.69063673414047,0.544852689532012));
#24908=CARTESIAN_POINT('Ctrl Pts',(97.7260715087293,1.69525640007447,0.530314471369937));
#24909=CARTESIAN_POINT('Ctrl Pts',(97.7255360236156,1.69762106372693,0.522695351808296));
#24910=CARTESIAN_POINT('Ctrl Pts',(97.7240922344492,1.7038913599639,0.50200051160188));
#24911=CARTESIAN_POINT('Ctrl Pts',(97.7231894240966,1.70769786490648,0.488894989321775));
#24912=CARTESIAN_POINT('Ctrl Pts',(97.7179510521506,1.72907912288824,0.411982412822237));
#24913=CARTESIAN_POINT('Ctrl Pts',(97.7137830337753,1.74322969857604,0.347269867565681));
#24914=CARTESIAN_POINT('Ctrl Pts',(97.7028272905171,1.77125343325277,0.172937823174047));
#24915=CARTESIAN_POINT('Ctrl Pts',(97.6961636456077,1.77856389059651,0.0626439766106631));
#24916=CARTESIAN_POINT('Ctrl Pts',(97.6892780533294,1.77561363837197,-0.0475422940912402));
#24917=CARTESIAN_POINT('Ctrl Pts',(97.5395352881717,1.77561363837197,-0.0475422940912293));
#24918=CARTESIAN_POINT('Ctrl Pts',(97.5419371591145,1.77663884788498,-0.00925268210916231));
#24919=CARTESIAN_POINT('Ctrl Pts',(97.5443657489703,1.77642598817633,0.0290864244276453));
#24920=CARTESIAN_POINT('Ctrl Pts',(97.5485161025327,1.77397510500667,0.0936151268840668));
#24921=CARTESIAN_POINT('Ctrl Pts',(97.5502168588313,1.77240010659219,0.11978820531831));
#24922=CARTESIAN_POINT('Ctrl Pts',(97.5529909444832,1.76892359461123,0.161965152295464));
#24923=CARTESIAN_POINT('Ctrl Pts',(97.5540530881059,1.76738253788206,0.17799531035738));
#24924=CARTESIAN_POINT('Ctrl Pts',(97.5559608844456,1.76424373587094,0.20656175374763));
#24925=CARTESIAN_POINT('Ctrl Pts',(97.5568038472848,1.76272974329664,0.219106265535949));
#24926=CARTESIAN_POINT('Ctrl Pts',(97.5586047728816,1.75922729330079,0.245735003006639));
#24927=CARTESIAN_POINT('Ctrl Pts',(97.5595638059636,1.75720324726604,0.259813564836092));
#24928=CARTESIAN_POINT('Ctrl Pts',(97.5621876949148,1.75123713904399,0.298046071965117));
#24929=CARTESIAN_POINT('Ctrl Pts',(97.563862850041,1.74696473512794,0.322144514392271));
#24930=CARTESIAN_POINT('Ctrl Pts',(97.5676359893372,1.73632160857712,0.375712700358774));
#24931=CARTESIAN_POINT('Ctrl Pts',(97.5697413781647,1.72969579651495,0.405123473296547));
#24932=CARTESIAN_POINT('Ctrl Pts',(97.5767108102229,1.70553644330522,0.500922401396418));
#24933=CARTESIAN_POINT('Ctrl Pts',(97.5816592184252,1.6849036034178,0.566459204399034));
#24934=CARTESIAN_POINT('Ctrl Pts',(97.5943815227014,1.62288313963923,0.729766755464741));
#24935=CARTESIAN_POINT('Ctrl Pts',(97.6022100834227,1.57643155989748,0.825332716883103));
#24936=CARTESIAN_POINT('Ctrl Pts',(97.6119127418899,1.50616454494463,0.94204207464389));
#24937=CARTESIAN_POINT('Ctrl Pts',(97.6140373124276,1.48994008014055,0.967498693342539));
#24938=CARTESIAN_POINT('Ctrl Pts',(97.6168904853991,1.46689745526781,1.00169760258894));
#24939=CARTESIAN_POINT('Ctrl Pts',(97.6176503194918,1.4606356450365,1.01080648965644));
#24940=CARTESIAN_POINT('Ctrl Pts',(97.6188580289242,1.45047475921969,1.02529564855163));
#24941=CARTESIAN_POINT('Ctrl Pts',(97.6193093973346,1.44662994089237,1.03071335098042));
#24942=CARTESIAN_POINT('Ctrl Pts',(97.6202677494203,1.43836332744599,1.0422243892309));
#24943=CARTESIAN_POINT('Ctrl Pts',(97.6207741207522,1.43393298470018,1.04831147081946));
#24944=CARTESIAN_POINT('Ctrl Pts',(97.6220676914719,1.42245863229558,1.06386783915769));
#24945=CARTESIAN_POINT('Ctrl Pts',(97.6228511360397,1.41535857672785,1.0732956059689));
#24946=CARTESIAN_POINT('Ctrl Pts',(97.6262364311107,1.38404880857153,1.11401903865881));
#24947=CARTESIAN_POINT('Ctrl Pts',(97.6287796051157,1.35888937072073,1.14457403951826));
#24948=CARTESIAN_POINT('Ctrl Pts',(97.6363732945961,1.27954562341276,1.23462492415807));
#24949=CARTESIAN_POINT('Ctrl Pts',(97.6412942118059,1.22232038627018,1.29130565102304));
#24950=CARTESIAN_POINT('Ctrl Pts',(97.6528943333001,1.07933979279307,1.41487324220862));
#24951=CARTESIAN_POINT('Ctrl Pts',(97.6595738775348,0.990912780022458,1.47815053604306));
#24952=CARTESIAN_POINT('Ctrl Pts',(97.6681462996586,0.876053427730697,1.54537983734966));
#24953=CARTESIAN_POINT('Ctrl Pts',(97.669743790925,0.854581734495018,1.55735622601384));
#24954=CARTESIAN_POINT('Ctrl Pts',(97.6723829283067,0.819058799598392,1.57621420620339));
#24955=CARTESIAN_POINT('Ctrl Pts',(97.6734151429244,0.805152563404083,1.58336283415792));
#24956=CARTESIAN_POINT('Ctrl Pts',(97.6752905940369,0.779876724830942,1.59593703245233));
#24957=CARTESIAN_POINT('Ctrl Pts',(97.6761315061215,0.768540221872781,1.60142706071519));
#24958=CARTESIAN_POINT('Ctrl Pts',(97.6779519523262,0.743997947403623,1.61299175144776));
#24959=CARTESIAN_POINT('Ctrl Pts',(97.6789328194399,0.730774156273614,1.61902577082223));
#24960=CARTESIAN_POINT('Ctrl Pts',(97.6816827530199,0.69370992947995,1.63539159451465));
#24961=CARTESIAN_POINT('Ctrl Pts',(97.6834638575235,0.66971547610311,1.6453632395989));
#24962=CARTESIAN_POINT('Ctrl Pts',(97.6912067650428,0.565507598330987,1.68601301631867));
#24963=CARTESIAN_POINT('Ctrl Pts',(97.6973376590116,0.483356649309191,1.7113741070999));
#24964=CARTESIAN_POINT('Ctrl Pts',(97.7133949114326,0.267890982706294,1.76113600589286));
#24965=CARTESIAN_POINT('Ctrl Pts',(97.7234461675429,0.133029388472,1.7764209467011));
#24966=CARTESIAN_POINT('Ctrl Pts',(97.734130235588,-0.0195114170905297,
1.77622658066348));
#24967=CARTESIAN_POINT('Ctrl Pts',(97.7353277997537,-0.0367591355060871,
1.77595337285126));
#24968=CARTESIAN_POINT('Ctrl Pts',(97.7371085722954,-0.0626713220210358,
1.77516523550523));
#24969=CARTESIAN_POINT('Ctrl Pts',(97.7377012095291,-0.0713399088181698,
1.7748380019945));
#24970=CARTESIAN_POINT('Ctrl Pts',(97.7387246484473,-0.0863944557493178,
1.77415922513816));
#24971=CARTESIAN_POINT('Ctrl Pts',(97.7391569976615,-0.0927812395864988,
1.7738366900193));
#24972=CARTESIAN_POINT('Ctrl Pts',(97.7401796429339,-0.107951766937579,
1.77298840974542));
#24973=CARTESIAN_POINT('Ctrl Pts',(97.7407682320153,-0.116733514956201,
1.77243188297211));
#24974=CARTESIAN_POINT('Ctrl Pts',(97.7425430882662,-0.143353011900473,
1.77054621837499));
#24975=CARTESIAN_POINT('Ctrl Pts',(97.7437187554771,-0.161175761214322,
1.76901284098851));
#24976=CARTESIAN_POINT('Ctrl Pts',(97.7496638677273,-0.252072048401022,
1.75980737631326));
#24977=CARTESIAN_POINT('Ctrl Pts',(97.7542443637918,-0.324649670041035,
1.74787507905684));
#24978=CARTESIAN_POINT('Ctrl Pts',(97.7672302606924,-0.529853785421857,
1.70090969337469));
#24979=CARTESIAN_POINT('Ctrl Pts',(97.7755096034912,-0.659424547624919,
1.65499112923024));
#24980=CARTESIAN_POINT('Ctrl Pts',(97.7863282871474,-0.811013741753595,
1.58061211328096));
#24981=CARTESIAN_POINT('Ctrl Pts',(97.7883909653162,-0.83921574793287,1.56582076550653));
#24982=CARTESIAN_POINT('Ctrl Pts',(97.7915089503022,-0.880690907666014,
1.54262552864903));
#24983=CARTESIAN_POINT('Ctrl Pts',(97.7925441365659,-0.894275778080294,
1.53479014947032));
#24984=CARTESIAN_POINT('Ctrl Pts',(97.7944227449241,-0.918584233923626,
1.52033739752042));
#24985=CARTESIAN_POINT('Ctrl Pts',(97.7952638062974,-0.92934464196915,1.51378377567218));
#24986=CARTESIAN_POINT('Ctrl Pts',(97.7970820480227,-0.952338182849639,
1.49944200697914));
#24987=CARTESIAN_POINT('Ctrl Pts',(97.7980605332358,-0.964547406860139,
1.4916174526218));
#24988=CARTESIAN_POINT('Ctrl Pts',(97.8007966202541,-0.998222518607995,
1.46944967161701));
#24989=CARTESIAN_POINT('Ctrl Pts',(97.8025660632571,-1.01947281200129,1.45478713133355));
#24990=CARTESIAN_POINT('Ctrl Pts',(97.8102111703715,-1.10900676781338,1.39008420687031));
#24991=CARTESIAN_POINT('Ctrl Pts',(97.8162508842426,-1.17397655159482,1.33566671001694));
#24992=CARTESIAN_POINT('Ctrl Pts',(97.831824961299,-1.32823187249575,1.18648789955951));
#24993=CARTESIAN_POINT('Ctrl Pts',(97.8414719049959,-1.41145456906662,1.08616346200528));
#24994=CARTESIAN_POINT('Ctrl Pts',(97.8521686221026,-1.49496269204481,0.959491499160685));
#24995=CARTESIAN_POINT('Ctrl Pts',(97.8536871265767,-1.50660326010684,0.941107916194747));
#24996=CARTESIAN_POINT('Ctrl Pts',(97.8558335719247,-1.52278578444251,0.914481207540025));
#24997=CARTESIAN_POINT('Ctrl Pts',(97.8564774304237,-1.5276041168009,0.906409453027667));
#24998=CARTESIAN_POINT('Ctrl Pts',(97.8576029567433,-1.53596740339845,0.892142997385941));
#24999=CARTESIAN_POINT('Ctrl Pts',(97.8580862998257,-1.53953943476725,0.885964631158831));
#25000=CARTESIAN_POINT('Ctrl Pts',(97.8591330234127,-1.54723311129706,0.872470208562674));
#25001=CARTESIAN_POINT('Ctrl Pts',(97.8596954999529,-1.55134022588294,0.865146274506095));
#25002=CARTESIAN_POINT('Ctrl Pts',(97.8613119503521,-1.56305815395625,0.843898718956846));
#25003=CARTESIAN_POINT('Ctrl Pts',(97.8623579165958,-1.57053475409258,0.829901481934332));
#25004=CARTESIAN_POINT('Ctrl Pts',(97.8647496378755,-1.58735257787546,0.797374665358724));
#25005=CARTESIAN_POINT('Ctrl Pts',(97.8660884833351,-1.59655883494904,0.77877758581373));
#25006=CARTESIAN_POINT('Ctrl Pts',(97.870710858708,-1.62750783232141,0.713402320511595));
#25007=CARTESIAN_POINT('Ctrl Pts',(97.873926323244,-1.64753850443317,0.665839480513909));
#25008=CARTESIAN_POINT('Ctrl Pts',(97.8848783852872,-1.70916172747797,0.499625976748066));
#25009=CARTESIAN_POINT('Ctrl Pts',(97.8924695072112,-1.74021948563971,0.377485083302912));
#25010=CARTESIAN_POINT('Ctrl Pts',(97.9030875904693,-1.76408419524224,0.211705443753069));
#25011=CARTESIAN_POINT('Ctrl Pts',(97.9057733424607,-1.76857821492427,0.170126171294622));
#25012=CARTESIAN_POINT('Ctrl Pts',(97.9096677871547,-1.77288887361713,0.110663428358246));
#25013=CARTESIAN_POINT('Ctrl Pts',(97.9108392467692,-1.773909438039,0.0928796004373038));
#25014=CARTESIAN_POINT('Ctrl Pts',(97.9128636357025,-1.77520132920039,0.0623448377334911));
#25015=CARTESIAN_POINT('Ctrl Pts',(97.9137124275394,-1.77560311037306,0.0496005839481933));
#25016=CARTESIAN_POINT('Ctrl Pts',(97.9154655531839,-1.77614671961305,0.0234054869731207));
#25017=CARTESIAN_POINT('Ctrl Pts',(97.9163703176002,-1.77627302615033,0.00995518283025552));
#25018=CARTESIAN_POINT('Ctrl Pts',(97.9186849738396,-1.77620568077855,-0.0242719771989726));
#25019=CARTESIAN_POINT('Ctrl Pts',(97.9201013790229,-1.77580025721604,-0.0450458849444988));
#25020=CARTESIAN_POINT('Ctrl Pts',(97.9265405207018,-1.77232872463862,-0.13868428019974));
#25021=CARTESIAN_POINT('Ctrl Pts',(97.9316887876581,-1.76514175187097,-0.211316225055452));
#25022=CARTESIAN_POINT('Ctrl Pts',(97.9449346441887,-1.73578302168071,-0.39303942032962));
#25023=CARTESIAN_POINT('Ctrl Pts',(97.9531457576869,-1.70778877041243,-0.500877128334812));
#25024=CARTESIAN_POINT('Ctrl Pts',(97.9650795568703,-1.65163205468216,-0.655781760095029));
#25025=CARTESIAN_POINT('Ctrl Pts',(97.968915515068,-1.63108616642553,-0.70533482489542));
#25026=CARTESIAN_POINT('Ctrl Pts',(97.9735688370383,-1.60268587940883,-0.765923460623624));
#25027=CARTESIAN_POINT('Ctrl Pts',(97.9744865151198,-1.59690867674238,-0.777896831412046));
#25028=CARTESIAN_POINT('Ctrl Pts',(97.9759338604355,-1.58750611361056,-0.796837531781246));
#25029=CARTESIAN_POINT('Ctrl Pts',(97.9764685573685,-1.58396816544437,-0.803847354723185));
#25030=CARTESIAN_POINT('Ctrl Pts',(97.9774951070953,-1.57704873424559,-0.81733391469048));
#25031=CARTESIAN_POINT('Ctrl Pts',(97.9779872989915,-1.57367361708345,-0.823813563396116));
#25032=CARTESIAN_POINT('Ctrl Pts',(97.9791940953441,-1.56525860227976,-0.839728521770535));
#25033=CARTESIAN_POINT('Ctrl Pts',(97.9799059040413,-1.56017316418026,-0.849139678885146));
#25034=CARTESIAN_POINT('Ctrl Pts',(97.9825799341316,-1.54061989690655,-0.884556362929399));
#25035=CARTESIAN_POINT('Ctrl Pts',(97.9845097940014,-1.52558350462171,-0.910244385996139));
#25036=CARTESIAN_POINT('Ctrl Pts',(97.9896095991787,-1.48358368731526,-0.978029371890028));
#25037=CARTESIAN_POINT('Ctrl Pts',(97.9927293480249,-1.45547641781806,-1.01938760093204));
#25038=CARTESIAN_POINT('Ctrl Pts',(98.0032291458754,-1.35419747768202,-1.15566727830361));
#25039=CARTESIAN_POINT('Ctrl Pts',(98.0104663588623,-1.27319245677475,-1.24434645446463));
#25040=CARTESIAN_POINT('Ctrl Pts',(98.0210429073214,-1.14817566122535,-1.35611586141513));
#25041=CARTESIAN_POINT('Ctrl Pts',(98.0241064242361,-1.1111995582421,-1.38657581964405));
#25042=CARTESIAN_POINT('Ctrl Pts',(98.0284505427962,-1.05811459247464,-1.42681756799562));
#25043=CARTESIAN_POINT('Ctrl Pts',(98.0296806365348,-1.04301128094236,-1.43789508901444));
#25044=CARTESIAN_POINT('Ctrl Pts',(98.0316968356135,-1.01816063391409,-1.45552424176401));
#25045=CARTESIAN_POINT('Ctrl Pts',(98.0324772860455,-1.00851827193534,-1.46222186370983));
#25046=CARTESIAN_POINT('Ctrl Pts',(98.0341296745711,-0.988060451087879,
-1.47613332941266));
#25047=CARTESIAN_POINT('Ctrl Pts',(98.0350023896007,-0.977230812993598,
-1.48332497577064));
#25048=CARTESIAN_POINT('Ctrl Pts',(98.0371277876091,-0.950803549775022,
-1.50045952808173));
#25049=CARTESIAN_POINT('Ctrl Pts',(98.038384960799,-0.93512794974577,-1.51027873521665));
#25050=CARTESIAN_POINT('Ctrl Pts',(98.0430764886706,-0.876489502391415,
-1.54574698986765));
#25051=CARTESIAN_POINT('Ctrl Pts',(98.0465664188311,-0.832605587350575,
-1.56981995490838));
#25052=CARTESIAN_POINT('Ctrl Pts',(98.0560740693701,-0.712387083414921,
-1.62930729761519));
#25053=CARTESIAN_POINT('Ctrl Pts',(98.0621874026624,-0.634459393613275,
-1.66120328586798));
#25054=CARTESIAN_POINT('Ctrl Pts',(98.0757177780561,-0.458646834427033,
-1.71898311839709));
#25055=CARTESIAN_POINT('Ctrl Pts',(98.0831285851693,-0.360198599004165,
-1.74227445631536));
#25056=CARTESIAN_POINT('Ctrl Pts',(98.0914517314965,-0.242741857388283,
-1.75967480493606));
#25057=CARTESIAN_POINT('Ctrl Pts',(98.0926847333336,-0.225147330882121,
-1.76201241987327));
#25058=CARTESIAN_POINT('Ctrl Pts',(98.0945071691658,-0.198807964918679,
-1.7651108757947));
#25059=CARTESIAN_POINT('Ctrl Pts',(98.0951066685777,-0.190088314238388,
-1.76607119102596));
#25060=CARTESIAN_POINT('Ctrl Pts',(98.0961850670182,-0.174296457946805,
-1.76769206889822));
#25061=CARTESIAN_POINT('Ctrl Pts',(98.0966651275992,-0.167227086390418,
-1.76837485033131));
#25062=CARTESIAN_POINT('Ctrl Pts',(98.097752993627,-0.151118188660109,-1.76983322932378));
#25063=CARTESIAN_POINT('Ctrl Pts',(98.0983593191796,-0.142076601695277,
-1.77058199888018));
#25064=CARTESIAN_POINT('Ctrl Pts',(98.1002466688599,-0.113749657320795,
-1.772709475433));
#25065=CARTESIAN_POINT('Ctrl Pts',(98.1015150361185,-0.0944465585079882,
-1.77384266246222));
#25066=CARTESIAN_POINT('Ctrl Pts',(98.1045222522783,-0.0481594669893906,
-1.77580216400853));
#25067=CARTESIAN_POINT('Ctrl Pts',(98.106248123938,-0.0211671023189207,
-1.77632901463453));
#25068=CARTESIAN_POINT('Ctrl Pts',(98.1131176827226,0.0874387578623564,
-1.7759726596306));
#25069=CARTESIAN_POINT('Ctrl Pts',(98.1181067590892,0.168939285567786,-1.77008070089214));
#25070=CARTESIAN_POINT('Ctrl Pts',(98.1296836064541,0.35565029070981,-1.7435647268776));
#25071=CARTESIAN_POINT('Ctrl Pts',(98.1362722839938,0.459963614353038,-1.71899246435281));
#25072=CARTESIAN_POINT('Ctrl Pts',(98.144745109016,0.58476420014083,-1.67741466052494));
#25073=CARTESIAN_POINT('Ctrl Pts',(98.1463434532876,0.607935970934208,-1.66915633597266));
#25074=CARTESIAN_POINT('Ctrl Pts',(98.1489837074697,0.645547762443126,-1.65486457139248));
#25075=CARTESIAN_POINT('Ctrl Pts',(98.1500161719442,0.660093192022824,-1.64911661655065));
#25076=CARTESIAN_POINT('Ctrl Pts',(98.1518918880881,0.686212867529391,-1.63839391614542));
#25077=CARTESIAN_POINT('Ctrl Pts',(98.1527328122948,0.697813810165198,-1.63348663793392));
#25078=CARTESIAN_POINT('Ctrl Pts',(98.1545530709162,0.722684517020114,-1.62265287132497));
#25079=CARTESIAN_POINT('Ctrl Pts',(98.1555337359409,0.73593562315748,-1.61668611320359));
#25080=CARTESIAN_POINT('Ctrl Pts',(98.1582824934228,0.772657363213013,-1.59960588896563));
#25081=CARTESIAN_POINT('Ctrl Pts',(98.1600626071388,0.795958889960783,-1.58813970484989));
#25082=CARTESIAN_POINT('Ctrl Pts',(98.1677971655269,0.895109510548429,-1.53661958927264));
#25083=CARTESIAN_POINT('Ctrl Pts',(98.1739202673956,0.968244157993132,-1.4916166768251));
#25084=CARTESIAN_POINT('Ctrl Pts',(98.1899829822579,1.14777658438383,-1.36236033822119));
#25085=CARTESIAN_POINT('Ctrl Pts',(98.2000488329196,1.24830444035904,-1.27088763640709));
#25086=CARTESIAN_POINT('Ctrl Pts',(98.2107428969953,1.34878504245925,-1.15591487250569));
#25087=CARTESIAN_POINT('Ctrl Pts',(98.2119378289671,1.35992248902994,-1.14279095291831));
#25088=CARTESIAN_POINT('Ctrl Pts',(98.2137155016879,1.37637927370779,-1.12281756133547));
#25089=CARTESIAN_POINT('Ctrl Pts',(98.2143076247235,1.38184174525249,-1.11608807007254));
#25090=CARTESIAN_POINT('Ctrl Pts',(98.2153305709726,1.39124895350104,-1.1043239163556));
#25091=CARTESIAN_POINT('Ctrl Pts',(98.2157629355758,1.39521596198389,-1.09930768459222));
#25092=CARTESIAN_POINT('Ctrl Pts',(98.2167861113364,1.4045815147121,-1.08733269592127));
#25093=CARTESIAN_POINT('Ctrl Pts',(98.2173752093448,1.40995550491436,-1.0803550830565));
#25094=CARTESIAN_POINT('Ctrl Pts',(98.2191532341675,1.42611049970892,-1.05905348993811));
#25095=CARTESIAN_POINT('Ctrl Pts',(98.2203315055686,1.43672712406474,-1.04460551570994));
#25096=CARTESIAN_POINT('Ctrl Pts',(98.2263036644115,1.48994984101678,-0.969828857736916));
#25097=CARTESIAN_POINT('Ctrl Pts',(98.2309066892802,1.5289865771356,-0.90703968983351));
#25098=CARTESIAN_POINT('Ctrl Pts',(98.2439885611737,1.6295265351328,-0.720287164590067));
#25099=CARTESIAN_POINT('Ctrl Pts',(98.2523414160577,1.68061428677739,-0.591357193237791));
#25100=CARTESIAN_POINT('Ctrl Pts',(98.2631585769089,1.72407792782382,-0.42842104542671));
#25101=CARTESIAN_POINT('Ctrl Pts',(98.2651305105155,1.73116113799823,-0.398836096408877));
#25102=CARTESIAN_POINT('Ctrl Pts',(98.2681508041026,1.74072437027604,-0.353816861656476));
#25103=CARTESIAN_POINT('Ctrl Pts',(98.2691813075371,1.74376626902148,-0.338506835867741));
#25104=CARTESIAN_POINT('Ctrl Pts',(98.2710549465546,1.74889721030061,-0.310775194624514));
#25105=CARTESIAN_POINT('Ctrl Pts',(98.2718957786435,1.75105667158789,-0.298367546198805));
#25106=CARTESIAN_POINT('Ctrl Pts',(98.2737175236098,1.75542703886347,-0.271572877420098));
#25107=CARTESIAN_POINT('Ctrl Pts',(98.2746997859108,1.7575933920722,-0.25717963111573));
#25108=CARTESIAN_POINT('Ctrl Pts',(98.2774578426196,1.76314687979346,-0.216926914012553));
#25109=CARTESIAN_POINT('Ctrl Pts',(98.2792457912219,1.7661416168894,-0.191017980664657));
#25110=CARTESIAN_POINT('Ctrl Pts',(98.2837696300757,1.77221356599926,-0.12595650345143));
#25111=CARTESIAN_POINT('Ctrl Pts',(98.2865256431726,1.77456345838068,-0.0867645056172716));
#25112=CARTESIAN_POINT('Ctrl Pts',(98.289313862947,1.77561363837197,-0.0475422940912524));
#25113=CARTESIAN_POINT('Origin',(88.3562164250559,0.,0.));
#25114=CARTESIAN_POINT('',(99.1886897733872,1.77561363837197,-0.04754229409124));
#25115=CARTESIAN_POINT('',(99.0420054636133,1.77561363839331,-0.0475422932941635));
#25116=CARTESIAN_POINT('',(88.3562164250559,1.77561363837197,-0.0475422940912398));
#25117=CARTESIAN_POINT('Ctrl Pts',(99.1886897733872,1.77561363837197,-0.0475422940912343));
#25118=CARTESIAN_POINT('Ctrl Pts',(99.1853655918391,1.7743934007775,-0.0931158314270797));
#25119=CARTESIAN_POINT('Ctrl Pts',(99.1820232071228,1.77141824310023,-0.138656366478061));
#25120=CARTESIAN_POINT('Ctrl Pts',(99.1747180039858,1.76105271532418,-0.238147712229466));
#25121=CARTESIAN_POINT('Ctrl Pts',(99.1707654191669,1.75293685978064,-0.291948735364658));
#25122=CARTESIAN_POINT('Ctrl Pts',(99.1646454542468,1.73624645399278,-0.376168724526229));
#25123=CARTESIAN_POINT('Ctrl Pts',(99.1624287111429,1.7293081351142,-0.406876298464051));
#25124=CARTESIAN_POINT('Ctrl Pts',(99.1594918742787,1.71885314255375,-0.448027341126179));
#25125=CARTESIAN_POINT('Ctrl Pts',(99.158737245475,1.71605069849231,-0.458644349977841));
#25126=CARTESIAN_POINT('Ctrl Pts',(99.1574823386392,1.71119192270817,-0.476383458904964));
#25127=CARTESIAN_POINT('Ctrl Pts',(99.1569791217336,1.70918916654739,-0.483519800167071));
#25128=CARTESIAN_POINT('Ctrl Pts',(99.1559464361303,1.7049653206176,-0.498216216129109));
#25129=CARTESIAN_POINT('Ctrl Pts',(99.1554172951155,1.70273850954039,-0.50577437332868));
#25130=CARTESIAN_POINT('Ctrl Pts',(99.1540095123898,1.69664847473252,-0.525948761124122));
#25131=CARTESIAN_POINT('Ctrl Pts',(99.1531359076543,1.69269476578993,-0.538537465406394));
#25132=CARTESIAN_POINT('Ctrl Pts',(99.1489103294804,1.67273655458295,-0.599692596467958));
#25133=CARTESIAN_POINT('Ctrl Pts',(99.145656479497,1.65477875901909,-0.647601022024729));
#25134=CARTESIAN_POINT('Ctrl Pts',(99.1322318050646,1.57092282876405,-0.844939786562546));
#25135=CARTESIAN_POINT('Ctrl Pts',(99.1225267294456,1.48665883891865,-0.985682789500896));
#25136=CARTESIAN_POINT('Ctrl Pts',(99.1098879580792,1.36269877248474,-1.13987296787201));
#25137=CARTESIAN_POINT('Ctrl Pts',(99.1076543331006,1.34026564081712,-1.16616726365281));
#25138=CARTESIAN_POINT('Ctrl Pts',(99.1043235309985,1.30616558520151,-1.20385222887757));
#25139=CARTESIAN_POINT('Ctrl Pts',(99.1032506721229,1.29508524292166,-1.21576433128528));
#25140=CARTESIAN_POINT('Ctrl Pts',(99.1013236362932,1.27502321056714,-1.2367468454062));
#25141=CARTESIAN_POINT('Ctrl Pts',(99.1004722067142,1.26610431724749,-1.24587591290242));
#25142=CARTESIAN_POINT('Ctrl Pts',(99.0986529540769,1.24693680553999,-1.265076724189));
#25143=CARTESIAN_POINT('Ctrl Pts',(99.097684037869,1.23666284915556,-1.27512175554073));
#25144=CARTESIAN_POINT('Ctrl Pts',(99.0950316486968,1.20836861635364,-1.30212192890378));
#25145=CARTESIAN_POINT('Ctrl Pts',(99.0933376417343,1.19011471043686,-1.31882640973637));
#25146=CARTESIAN_POINT('Ctrl Pts',(99.0816487282209,1.06298059048463,-1.43037995726261));
#25147=CARTESIAN_POINT('Ctrl Pts',(99.0711107372911,0.943252698267116,-1.51200966178706));
#25148=CARTESIAN_POINT('Ctrl Pts',(99.0549142438954,0.746329323859891,-1.61370069789504));
#25149=CARTESIAN_POINT('Ctrl Pts',(99.0492939992146,0.675409699749159,-1.64464627735572));
#25150=CARTESIAN_POINT('Ctrl Pts',(99.0425823107762,0.585426168804902,-1.67710382076618));
#25151=CARTESIAN_POINT('Ctrl Pts',(99.0413060112466,0.568062250892884,-1.68306457681726));
#25152=CARTESIAN_POINT('Ctrl Pts',(99.0394292726399,0.542107551231169,-1.69152694583775));
#25153=CARTESIAN_POINT('Ctrl Pts',(99.0388180051892,0.533585843355805,-1.69423438816787));
#25154=CARTESIAN_POINT('Ctrl Pts',(99.0377712990078,0.518869680928439,-1.69878782853164));
#25155=CARTESIAN_POINT('Ctrl Pts',(99.0373341366804,0.51268520247532,-1.70066449341263));
#25156=CARTESIAN_POINT('Ctrl Pts',(99.0363114049782,0.49812675834041,-1.70499558196026));
#25157=CARTESIAN_POINT('Ctrl Pts',(99.0357274421577,0.489744787357734,-1.70742210749768));
#25158=CARTESIAN_POINT('Ctrl Pts',(99.0340342100576,0.465250652675802,-1.7143177803379));
#25159=CARTESIAN_POINT('Ctrl Pts',(99.0329338610926,0.449092359875985,-1.71862146028356));
#25160=CARTESIAN_POINT('Ctrl Pts',(99.0243800590873,0.321829100888745,-1.75059986292592));
#25161=CARTESIAN_POINT('Ctrl Pts',(99.0174098392056,0.208329635111639,-1.76770467022071));
#25162=CARTESIAN_POINT('Ctrl Pts',(99.0043488632174,-0.00410467531662812,
-1.77895784161103));
#25163=CARTESIAN_POINT('Ctrl Pts',(98.9982963472337,-0.102422050787166,
-1.77601094703713));
#25164=CARTESIAN_POINT('Ctrl Pts',(98.9899907356909,-0.231164989801637,
-1.76142310901206));
#25165=CARTESIAN_POINT('Ctrl Pts',(98.9879573511447,-0.26224242541558,-1.75706497866967));
#25166=CARTESIAN_POINT('Ctrl Pts',(98.9848687432149,-0.308661201271373,
-1.74929657074224));
#25167=CARTESIAN_POINT('Ctrl Pts',(98.983832873189,-0.324100285114179,-1.74650199209836));
#25168=CARTESIAN_POINT('Ctrl Pts',(98.9819455264714,-0.351983166697774,
-1.74107255821595));
#25169=CARTESIAN_POINT('Ctrl Pts',(98.981096339101,-0.364439659402339,-1.73850784375318));
#25170=CARTESIAN_POINT('Ctrl Pts',(98.9792517110055,-0.391298986780564,
-1.73267632803631));
#25171=CARTESIAN_POINT('Ctrl Pts',(98.9782548407113,-0.405690677627047,
-1.7293632371168));
#25172=CARTESIAN_POINT('Ctrl Pts',(98.9754905083115,-0.445248864144231,
-1.71973564615285));
#25173=CARTESIAN_POINT('Ctrl Pts',(98.973711244928,-0.470320023236342,-1.7130488012569));
#25174=CARTESIAN_POINT('Ctrl Pts',(98.9627560009343,-0.62225491264947,-1.66893886346217));
#25175=CARTESIAN_POINT('Ctrl Pts',(98.9531381926924,-0.744737609617128,
-1.61799625190002));
#25176=CARTESIAN_POINT('Ctrl Pts',(98.9387751744068,-0.916557642621267,
-1.52286089100711));
#25177=CARTESIAN_POINT('Ctrl Pts',(98.9340881646006,-0.970982670593367,
-1.48875005448321));
#25178=CARTESIAN_POINT('Ctrl Pts',(98.9270063664742,-1.05193503502289,-1.4316814844162));
#25179=CARTESIAN_POINT('Ctrl Pts',(98.9245446169095,-1.07983066464143,-1.41076054225632));
#25180=CARTESIAN_POINT('Ctrl Pts',(98.9213426083941,-1.11599475049936,-1.38193679851596));
#25181=CARTESIAN_POINT('Ctrl Pts',(98.9205597403517,-1.12482691845868,-1.37475744002252));
#25182=CARTESIAN_POINT('Ctrl Pts',(98.9192712337831,-1.13935703203509,-1.36271263796874));
#25183=CARTESIAN_POINT('Ctrl Pts',(98.9187623207169,-1.14509418747203,-1.35789524235546));
#25184=CARTESIAN_POINT('Ctrl Pts',(98.9177317861651,-1.15671157779988,-1.34801431649525));
#25185=CARTESIAN_POINT('Ctrl Pts',(98.9172103550533,-1.16258940881228,-1.34294830281267));
#25186=CARTESIAN_POINT('Ctrl Pts',(98.9158466032465,-1.17795474137115,-1.32952866687338));
#25187=CARTESIAN_POINT('Ctrl Pts',(98.9150087796622,-1.18738679453287,-1.32111183162366));
#25188=CARTESIAN_POINT('Ctrl Pts',(98.9112792988069,-1.22928902317129,-1.28290842335939));
#25189=CARTESIAN_POINT('Ctrl Pts',(98.908459905395,-1.2607366513882,-1.25201809917143));
#25190=CARTESIAN_POINT('Ctrl Pts',(98.8996736473734,-1.35657216437321,-1.15060380264404));
#25191=CARTESIAN_POINT('Ctrl Pts',(98.8938787514653,-1.41644237731922,-1.07604378091271));
#25192=CARTESIAN_POINT('Ctrl Pts',(98.8825364292769,-1.51986205985886,-0.923560528793251));
#25193=CARTESIAN_POINT('Ctrl Pts',(98.8770157542252,-1.56410841159947,-0.846467393317558));
#25194=CARTESIAN_POINT('Ctrl Pts',(98.8695858986433,-1.61382738017507,-0.742513357050467));
#25195=CARTESIAN_POINT('Ctrl Pts',(98.8678626619265,-1.62471391625138,-0.718379753274194));
#25196=CARTESIAN_POINT('Ctrl Pts',(98.86515232877,-1.64081042075584,-0.680457262471034));
#25197=CARTESIAN_POINT('Ctrl Pts',(98.8641779750259,-1.64639525545746,-0.666830985903728));
#25198=CARTESIAN_POINT('Ctrl Pts',(98.8623512376158,-1.65648721988568,-0.641308006905735));
#25199=CARTESIAN_POINT('Ctrl Pts',(98.8615003672752,-1.66103724594756,-0.62942920365116));
#25200=CARTESIAN_POINT('Ctrl Pts',(98.8595867745885,-1.67093199307132,-0.602742203805938));
#25201=CARTESIAN_POINT('Ctrl Pts',(98.8585218429632,-1.6762081584955,-0.587909917617987));
#25202=CARTESIAN_POINT('Ctrl Pts',(98.8557712079912,-1.68924429291163,-0.549660184306032));
#25203=CARTESIAN_POINT('Ctrl Pts',(98.8540762122415,-1.69671459747118,-0.526148332548572));
#25204=CARTESIAN_POINT('Ctrl Pts',(98.8448155523712,-1.7344946103781,-0.398055064325833));
#25205=CARTESIAN_POINT('Ctrl Pts',(98.8369629025161,-1.75562411564626,-0.291026234724324));
#25206=CARTESIAN_POINT('Ctrl Pts',(98.8231721092441,-1.77504843875658,-0.103236649659238));
#25207=CARTESIAN_POINT('Ctrl Pts',(98.8173006873,-1.77789622299953,-0.0232520401958028));
#25208=CARTESIAN_POINT('Ctrl Pts',(98.8096424742066,-1.77449283939336,0.0833974388469762));
#25209=CARTESIAN_POINT('Ctrl Pts',(98.8077385175066,-1.77303522794508,0.110119037685076));
#25210=CARTESIAN_POINT('Ctrl Pts',(98.804506493651,-1.7694922730804,0.155985521807472));
#25211=CARTESIAN_POINT('Ctrl Pts',(98.8031670754739,-1.76769841838572,0.17514783552763));
#25212=CARTESIAN_POINT('Ctrl Pts',(98.8012166407239,-1.7645971226372,0.203332308239764));
#25213=CARTESIAN_POINT('Ctrl Pts',(98.8005935828458,-1.76353118416357,0.212378917090293));
#25214=CARTESIAN_POINT('Ctrl Pts',(98.7994866983602,-1.76150141464823,0.228535103057142));
#25215=CARTESIAN_POINT('Ctrl Pts',(98.7990014777767,-1.76056405615017,0.235647483427507));
#25216=CARTESIAN_POINT('Ctrl Pts',(98.7979180495305,-1.75836380205932,0.251595827902148));
#25217=CARTESIAN_POINT('Ctrl Pts',(98.7973211495345,-1.75707737481331,0.260428163777265));
#25218=CARTESIAN_POINT('Ctrl Pts',(98.7955128630197,-1.75295480552192,0.287310531903416));
#25219=CARTESIAN_POINT('Ctrl Pts',(98.7943125660607,-1.74990659700875,0.305327459531161));
#25220=CARTESIAN_POINT('Ctrl Pts',(98.7874779139404,-1.73077690356379,0.408674420337282));
#25221=CARTESIAN_POINT('Ctrl Pts',(98.7821099263512,-1.70873179509717,0.492790724815104));
#25222=CARTESIAN_POINT('Ctrl Pts',(98.7716504320384,-1.65365588455882,0.653777184477575));
#25223=CARTESIAN_POINT('Ctrl Pts',(98.7665682559406,-1.62118309839323,0.730593686956729));
#25224=CARTESIAN_POINT('Ctrl Pts',(98.7587953743425,-1.56484439991561,0.841433679805118));
#25225=CARTESIAN_POINT('Ctrl Pts',(98.7562027206278,-1.54498544507029,0.877364388479768));
#25226=CARTESIAN_POINT('Ctrl Pts',(98.7515861669163,-1.50800319683622,0.939120824538004));
#25227=CARTESIAN_POINT('Ctrl Pts',(98.7495801744132,-1.4914153587427,0.96524691523214));
#25228=CARTESIAN_POINT('Ctrl Pts',(98.7465248642275,-1.46544750786853,1.00387810556305));
#25229=CARTESIAN_POINT('Ctrl Pts',(98.7454942651578,-1.4565705097325,1.0167152862802));
#25230=CARTESIAN_POINT('Ctrl Pts',(98.7436124682416,-1.4401579709312,1.0397935837147));
#25231=CARTESIAN_POINT('Ctrl Pts',(98.7427634949703,-1.43267936766312,1.05007404166609));
#25232=CARTESIAN_POINT('Ctrl Pts',(98.7409146461137,-1.4162376790882,1.07217297615569));
#25233=CARTESIAN_POINT('Ctrl Pts',(98.7399132876168,-1.40723567697853,1.0839611527235));
#25234=CARTESIAN_POINT('Ctrl Pts',(98.7371236904087,-1.38189798586762,1.11629336927533));
#25235=CARTESIAN_POINT('Ctrl Pts',(98.7353232936643,-1.36525354271101,1.13658944457184));
#25236=CARTESIAN_POINT('Ctrl Pts',(98.7245622101405,-1.26410964732252,1.25449502180644));
#25237=CARTESIAN_POINT('Ctrl Pts',(98.7151838822325,-1.16963485109714,1.34300929100709));
#25238=CARTESIAN_POINT('Ctrl Pts',(98.7009129047559,-1.01358937622943,1.46015954330516));
#25239=CARTESIAN_POINT('Ctrl Pts',(98.696084047736,-0.95857742238463,1.49684986835111));
#25240=CARTESIAN_POINT('Ctrl Pts',(98.6888200224892,-0.871091029044569,
1.54839342678187));
#25241=CARTESIAN_POINT('Ctrl Pts',(98.6863143274156,-0.840000626976328,
1.56547792405233));
#25242=CARTESIAN_POINT('Ctrl Pts',(98.6830651927527,-0.798223280701308,
1.58683166103935));
#25243=CARTESIAN_POINT('Ctrl Pts',(98.6822776109989,-0.787978915687187,
1.59194358323487));
#25244=CARTESIAN_POINT('Ctrl Pts',(98.680983494902,-0.770938531780708,1.60024190665419));
#25245=CARTESIAN_POINT('Ctrl Pts',(98.6804736289704,-0.764170595658663,
1.60348485725573));
#25246=CARTESIAN_POINT('Ctrl Pts',(98.6795072361373,-0.751235177516634,
1.60958253944513));
#25247=CARTESIAN_POINT('Ctrl Pts',(98.6790502187828,-0.745071556700032,
1.61244492078025));
#25248=CARTESIAN_POINT('Ctrl Pts',(98.6778166922189,-0.728314711739129,
1.62011018794636));
#25249=CARTESIAN_POINT('Ctrl Pts',(98.6770442375694,-0.717690275736269,
1.62484461611598));
#25250=CARTESIAN_POINT('Ctrl Pts',(98.674027012129,-0.675712106864466,1.64305870571012));
#25251=CARTESIAN_POINT('Ctrl Pts',(98.6718247187761,-0.644017051319341,
1.65573885405461));
#25252=CARTESIAN_POINT('Ctrl Pts',(98.6631162420858,-0.515445484201801,
1.70292476970301));
#25253=CARTESIAN_POINT('Ctrl Pts',(98.6568762560695,-0.416015601717569,
1.72990498191401));
#25254=CARTESIAN_POINT('Ctrl Pts',(98.6448591896422,-0.223712728737859,
1.76453484334769));
#25255=CARTESIAN_POINT('Ctrl Pts',(98.6391163310975,-0.131489548701381,
1.77379208137029));
#25256=CARTESIAN_POINT('Ctrl Pts',(98.6314158825446,-0.0120159714731658,
1.77641397412405));
#25257=CARTESIAN_POINT('Ctrl Pts',(98.6296616920669,0.0149478827089522,
1.77639168728451));
#25258=CARTESIAN_POINT('Ctrl Pts',(98.6269134675092,0.056721081769153,1.77540603183595));
#25259=CARTESIAN_POINT('Ctrl Pts',(98.625932778585,0.0715371409881411,1.77487077672411));
#25260=CARTESIAN_POINT('Ctrl Pts',(98.6241002612597,0.0990427900830045,
1.7735321309148));
#25261=CARTESIAN_POINT('Ctrl Pts',(98.6232500284524,0.111733889720835,1.77277782506423));
#25262=CARTESIAN_POINT('Ctrl Pts',(98.6213458058649,0.139993132443401,1.77079356329233));
#25263=CARTESIAN_POINT('Ctrl Pts',(98.620289706387,0.155555192378052,1.76949441249334));
#25264=CARTESIAN_POINT('Ctrl Pts',(98.6171858477343,0.200956353272661,1.76510070444062));
#25265=CARTESIAN_POINT('Ctrl Pts',(98.6151211068252,0.230735346222123,1.76145535350444));
#25266=CARTESIAN_POINT('Ctrl Pts',(98.6033794876242,0.397640475646846,1.73671903822601));
#25267=CARTESIAN_POINT('Ctrl Pts',(98.593227490331,0.531999176174459,1.70037494881006));
#25268=CARTESIAN_POINT('Ctrl Pts',(98.5790893099674,0.711680908388488,1.62836936601019));
#25269=CARTESIAN_POINT('Ctrl Pts',(98.5750987581099,0.761657481554427,1.60560116400373));
#25270=CARTESIAN_POINT('Ctrl Pts',(98.568928291336,0.8386733296598,1.56610773033495));
#25271=CARTESIAN_POINT('Ctrl Pts',(98.5666981463312,0.866455525316215,1.5509098923693));
#25272=CARTESIAN_POINT('Ctrl Pts',(98.5637466923177,0.903327222458187,1.52943946103634));
#25273=CARTESIAN_POINT('Ctrl Pts',(98.5629904284223,0.912784591470168,1.52381410971773));
#25274=CARTESIAN_POINT('Ctrl Pts',(98.5617335720251,0.928527920055514,1.51425062890651));
#25275=CARTESIAN_POINT('Ctrl Pts',(98.5612300216202,0.934842494583412,1.51036041516676));
#25276=CARTESIAN_POINT('Ctrl Pts',(98.560197442476,0.947809300271062,1.50225948730427));
#25277=CARTESIAN_POINT('Ctrl Pts',(98.5596687334252,0.954458194486666,1.49804392389004));
#25278=CARTESIAN_POINT('Ctrl Pts',(98.5582635418187,0.972147243862521,1.48666304702944));
#25279=CARTESIAN_POINT('Ctrl Pts',(98.5573920627569,0.983136403498689,1.47941884425101));
#25280=CARTESIAN_POINT('Ctrl Pts',(98.5532051093773,1.03595757479437,1.44374988768768));
#25281=CARTESIAN_POINT('Ctrl Pts',(98.5499855428606,1.07664705352534,1.41366684949636));
#25282=CARTESIAN_POINT('Ctrl Pts',(98.5365686148749,1.24329277849515,1.2790849515194));
#25283=CARTESIAN_POINT('Ctrl Pts',(98.5268456739964,1.35576864060012,1.15919373416175));
#25284=CARTESIAN_POINT('Ctrl Pts',(98.5141753303012,1.47030673723865,0.997230721897223));
#25285=CARTESIAN_POINT('Ctrl Pts',(98.5119301891267,1.48952844472357,0.968284963338501));
#25286=CARTESIAN_POINT('Ctrl Pts',(98.5085854473844,1.51650398303549,0.924957011884526));
#25287=CARTESIAN_POINT('Ctrl Pts',(98.5075104643707,1.52492864688005,0.911000766669012));
#25288=CARTESIAN_POINT('Ctrl Pts',(98.5055810222647,1.53960661139219,0.885911136446451));
#25289=CARTESIAN_POINT('Ctrl Pts',(98.5047293358463,1.54593427384532,0.874822419612228));
#25290=CARTESIAN_POINT('Ctrl Pts',(98.5029110386238,1.55911957693626,0.851126404757805));
#25291=CARTESIAN_POINT('Ctrl Pts',(98.5019433509962,1.56594502415916,0.838502338871315));
#25292=CARTESIAN_POINT('Ctrl Pts',(98.499298271279,1.58407846727482,0.803969706712192));
#25293=CARTESIAN_POINT('Ctrl Pts',(98.49761044578,1.59508413231313,0.781906889647084));
#25294=CARTESIAN_POINT('Ctrl Pts',(98.4858863631611,1.66764272314306,0.628538722057488));
#25295=CARTESIAN_POINT('Ctrl Pts',(98.4753015316341,1.7133620134927,0.490375265286924));
#25296=CARTESIAN_POINT('Ctrl Pts',(98.4590902808865,1.75685440464913,0.272833814031389));
#25297=CARTESIAN_POINT('Ctrl Pts',(98.4535002958183,1.76701811105037,0.196532193408574));
#25298=CARTESIAN_POINT('Ctrl Pts',(98.4468199706563,1.77344041694632,0.101531418005063));
#25299=CARTESIAN_POINT('Ctrl Pts',(98.4455465498248,1.77439314168554,0.0832381253092255));
#25300=CARTESIAN_POINT('Ctrl Pts',(98.4436731452741,1.77538935398147,0.0560046241025156));
#25301=CARTESIAN_POINT('Ctrl Pts',(98.4430623886061,1.77564858790227,0.0470741658988919));
#25302=CARTESIAN_POINT('Ctrl Pts',(98.4420162058808,1.77597921489377,0.0316805725871297));
#25303=CARTESIAN_POINT('Ctrl Pts',(98.4415790622106,1.77608272802193,0.0252185935006792));
#25304=CARTESIAN_POINT('Ctrl Pts',(98.440555870741,1.77624318808995,0.0100232632241994));
#25305=CARTESIAN_POINT('Ctrl Pts',(98.4399714354593,1.77627100220953,0.00128988648284571));
#25306=CARTESIAN_POINT('Ctrl Pts',(98.4385008173595,1.7761783837321,-0.0208113540785626));
#25307=CARTESIAN_POINT('Ctrl Pts',(98.4376191380422,1.77597145713807,-0.0341784484187622));
#25308=CARTESIAN_POINT('Ctrl Pts',(98.4367443001643,1.77561363837182,-0.0475422940967033));
#25309=CARTESIAN_POINT('',(98.4811171438985,0.00162347919700848,1.77624925807593));
#25310=CARTESIAN_POINT('Ctrl Pts',(98.289313862947,1.77561363837197,-0.0475422940912524));
#25311=CARTESIAN_POINT('Ctrl Pts',(98.2926748518192,1.77687955123043,-0.000262873115973129));
#25312=CARTESIAN_POINT('Ctrl Pts',(98.2960828732913,1.77625693264144,0.0470604327664538));
#25313=CARTESIAN_POINT('Ctrl Pts',(98.3092516879989,1.76662997259377,0.228110696891337));
#25314=CARTESIAN_POINT('Ctrl Pts',(98.3192027038273,1.74440043006838,0.360673984676432));
#25315=CARTESIAN_POINT('Ctrl Pts',(98.3298177239441,1.70265328893669,0.506302355255301));
#25316=CARTESIAN_POINT('Ctrl Pts',(98.3310331350711,1.69758237990944,0.52305297849011));
#25317=CARTESIAN_POINT('Ctrl Pts',(98.332834906219,1.68961372689328,0.548037973578791));
#25318=CARTESIAN_POINT('Ctrl Pts',(98.3334310134548,1.68690168186181,0.556329839586212));
#25319=CARTESIAN_POINT('Ctrl Pts',(98.3344578002709,1.68209655016203,0.570662883572255));
#25320=CARTESIAN_POINT('Ctrl Pts',(98.3348900687355,1.68003183489243,0.576713072352935));
#25321=CARTESIAN_POINT('Ctrl Pts',(98.335909235951,1.67506457256116,0.591015444484796));
#25322=CARTESIAN_POINT('Ctrl Pts',(98.3364944684919,1.67213367977719,0.599257492989124));
#25323=CARTESIAN_POINT('Ctrl Pts',(98.33824851222,1.66311583413547,0.62403546039924));
#25324=CARTESIAN_POINT('Ctrl Pts',(98.3394070841259,1.65684340338447,0.640503339522243));
#25325=CARTESIAN_POINT('Ctrl Pts',(98.3451772684421,1.62406675285224,0.722850979244298));
#25326=CARTESIAN_POINT('Ctrl Pts',(98.3496120734622,1.59387121686358,0.787199528455292));
#25327=CARTESIAN_POINT('Ctrl Pts',(98.3619943555025,1.49795900545056,0.963303832718304));
#25328=CARTESIAN_POINT('Ctrl Pts',(98.3698167081504,1.42377010853301,1.06991244510049));
#25329=CARTESIAN_POINT('Ctrl Pts',(98.3804699594886,1.31370190167222,1.19611550347375));
#25330=CARTESIAN_POINT('Ctrl Pts',(98.3829148951586,1.28784252760183,1.22391432785782));
#25331=CARTESIAN_POINT('Ctrl Pts',(98.3864111018609,1.25019429420161,1.26187112190757));
#25332=CARTESIAN_POINT('Ctrl Pts',(98.3874311661815,1.23913127248095,1.2727364872564));
#25333=CARTESIAN_POINT('Ctrl Pts',(98.3893084125561,1.21863990764363,1.29234130997582));
#25334=CARTESIAN_POINT('Ctrl Pts',(98.3901635611303,1.20925614744861,1.30112598967335));
#25335=CARTESIAN_POINT('Ctrl Pts',(98.3919116788421,1.18997983046023,1.3187830089058));
#25336=CARTESIAN_POINT('Ctrl Pts',(98.3928048933193,1.18008142031832,1.32764771163769));
#25337=CARTESIAN_POINT('Ctrl Pts',(98.3937500890546,1.16955835449965,1.33686117729683));
#25338=CARTESIAN_POINT('Ctrl Pts',(98.3937973804396,1.16903172191039,1.33732172086906));
#25339=CARTESIAN_POINT('Ctrl Pts',(98.3938910820493,1.16798801740504,1.33823335952641));
#25340=CARTESIAN_POINT('Ctrl Pts',(98.3939374917743,1.1674709558828,1.33868446637692));
#25341=CARTESIAN_POINT('Ctrl Pts',(98.3940299924789,1.16644014107159,1.33958274238679));
#25342=CARTESIAN_POINT('Ctrl Pts',(98.3940760832672,1.16592639171338,1.34002991590023));
#25343=CARTESIAN_POINT('Ctrl Pts',(98.3955449320196,1.14955010418151,1.35426748302609));
#25344=CARTESIAN_POINT('Ctrl Pts',(98.396979267043,1.13344491347429,1.36777498861236));
#25345=CARTESIAN_POINT('Ctrl Pts',(98.4035806832206,1.058837064672,1.42812631167305));
#25346=CARTESIAN_POINT('Ctrl Pts',(98.4088804281883,0.99765300898167,1.47151843145206));
#25347=CARTESIAN_POINT('Ctrl Pts',(98.4214706820547,0.849054705011137,1.56336936999886));
#25348=CARTESIAN_POINT('Ctrl Pts',(98.4288226220731,0.759923363159647,1.60858088611291));
#25349=CARTESIAN_POINT('Ctrl Pts',(98.440494697446,0.611053310709455,1.66894721811466));
#25350=CARTESIAN_POINT('Ctrl Pts',(98.4448690506855,0.553485999450752,1.68891259510949));
#25351=CARTESIAN_POINT('Ctrl Pts',(98.4500574456642,0.48188554245696,1.70968912342778));
#25352=CARTESIAN_POINT('Ctrl Pts',(98.4510007887297,0.468725649094946,1.7133437685902));
#25353=CARTESIAN_POINT('Ctrl Pts',(98.4524789907407,0.447859275483054,1.71888016523592));
#25354=CARTESIAN_POINT('Ctrl Pts',(98.4530192363543,0.440180410349877,1.72086262253008));
#25355=CARTESIAN_POINT('Ctrl Pts',(98.4540488943388,0.425438818715921,1.72456333650106));
#25356=CARTESIAN_POINT('Ctrl Pts',(98.4545387242794,0.418378496097635,1.72628975722882));
#25357=CARTESIAN_POINT('Ctrl Pts',(98.4557293251382,0.40110642187058,1.73040101197066));
#25358=CARTESIAN_POINT('Ctrl Pts',(98.4564274755549,0.390883568340982,1.73273889357978));
#25359=CARTESIAN_POINT('Ctrl Pts',(98.457923829001,0.368784289121395,1.73758727588388));
#25360=CARTESIAN_POINT('Ctrl Pts',(98.4587204364205,0.356901554587099,1.7400668642479));
#25361=CARTESIAN_POINT('Ctrl Pts',(98.4670245891664,0.231918324213672,1.76481310706288));
#25362=CARTESIAN_POINT('Ctrl Pts',(98.4740375076626,0.116925795384379,1.77614387257846));
#25363=CARTESIAN_POINT('Ctrl Pts',(98.4811171438985,0.00162347919702141,
1.77624925807593));
#25364=CARTESIAN_POINT('Ctrl Pts',(98.4811171438985,0.00162347919766435,
1.77624925807593));
#25365=CARTESIAN_POINT('Ctrl Pts',(98.4875839157544,-0.103697436792226,
1.77634552064461));
#25366=CARTESIAN_POINT('Ctrl Pts',(98.494081006342,-0.208796193401722,1.76707590037909));
#25367=CARTESIAN_POINT('Ctrl Pts',(98.5020981984134,-0.331206729051687,
1.74520167397757));
#25368=CARTESIAN_POINT('Ctrl Pts',(98.5033345465983,-0.349899210184728,
1.74155025172625));
#25369=CARTESIAN_POINT('Ctrl Pts',(98.5054576915823,-0.381654194789689,
1.73481531090901));
#25370=CARTESIAN_POINT('Ctrl Pts',(98.5063397633945,-0.394747301001014,
1.73188297511));
#25371=CARTESIAN_POINT('Ctrl Pts',(98.5081044220591,-0.420732992364379,
1.72575323467924));
#25372=CARTESIAN_POINT('Ctrl Pts',(98.508986857412,-0.43362542444743,1.72255898384962));
#25373=CARTESIAN_POINT('Ctrl Pts',(98.5107328039029,-0.458925592904638,
1.71598854539845));
#25374=CARTESIAN_POINT('Ctrl Pts',(98.5115959674733,-0.471334902767029,
1.71262161089462));
#25375=CARTESIAN_POINT('Ctrl Pts',(98.513706922513,-0.501436778407503,1.7041023356231));
#25376=CARTESIAN_POINT('Ctrl Pts',(98.5149592350811,-0.519087499813065,
1.69880891680824));
#25377=CARTESIAN_POINT('Ctrl Pts',(98.5193533491707,-0.580281886891746,
1.67941411298376));
#25378=CARTESIAN_POINT('Ctrl Pts',(98.5225402361988,-0.623357159398503,
1.66390625594159));
#25379=CARTESIAN_POINT('Ctrl Pts',(98.5331483485892,-0.762482084685145,
1.60765805585683));
#25380=CARTESIAN_POINT('Ctrl Pts',(98.5407652104414,-0.855540222574703,
1.56012487059466));
#25381=CARTESIAN_POINT('Ctrl Pts',(98.5529661464366,-0.996886164596863,
1.47146092481033));
#25382=CARTESIAN_POINT('Ctrl Pts',(98.5575322656208,-1.04810136681483,1.43543152092562));
#25383=CARTESIAN_POINT('Ctrl Pts',(98.5644393845948,-1.12410865233419,1.37571986674328));
#25384=CARTESIAN_POINT('Ctrl Pts',(98.5668449705458,-1.15029743806007,1.3538986580067));
#25385=CARTESIAN_POINT('Ctrl Pts',(98.5699898124653,-1.18434131904986,1.32383089194837));
#25386=CARTESIAN_POINT('Ctrl Pts',(98.570769630895,-1.19276688433482,1.31624456962711));
#25387=CARTESIAN_POINT('Ctrl Pts',(98.5720510214666,-1.20659376044404,1.30355313468374));
#25388=CARTESIAN_POINT('Ctrl Pts',(98.5725558631913,-1.2120365933746,1.29849396643398));
#25389=CARTESIAN_POINT('Ctrl Pts',(98.5735753785123,-1.22302183098433,1.28815381981295));
#25390=CARTESIAN_POINT('Ctrl Pts',(98.5740898933287,-1.22856212945266,1.28287090629999));
#25391=CARTESIAN_POINT('Ctrl Pts',(98.5754300682774,-1.24297766284799,1.26894603370402));
#25392=CARTESIAN_POINT('Ctrl Pts',(98.576251438368,-1.25179713435195,1.2602465880456));
#25393=CARTESIAN_POINT('Ctrl Pts',(98.5798302854721,-1.29011325097555,1.22165277626801));
#25394=CARTESIAN_POINT('Ctrl Pts',(98.5825222048819,-1.31863773503365,1.1908076446268));
#25395=CARTESIAN_POINT('Ctrl Pts',(98.591290013983,-1.40931625978545,1.08549301844199));
#25396=CARTESIAN_POINT('Ctrl Pts',(98.5971759493595,-1.46646821425704,1.00694623045769));
#25397=CARTESIAN_POINT('Ctrl Pts',(98.6086676286214,-1.56360968666951,0.847490809877018));
#25398=CARTESIAN_POINT('Ctrl Pts',(98.614245295967,-1.60441542964787,0.7674401857532));
#25399=CARTESIAN_POINT('Ctrl Pts',(98.6217380132887,-1.64920890843683,0.660209009121993));
#25400=CARTESIAN_POINT('Ctrl Pts',(98.6234625044879,-1.65887208667197,0.635538543580224));
#25401=CARTESIAN_POINT('Ctrl Pts',(98.6261684087063,-1.67301255676996,0.596914874832605));
#25402=CARTESIAN_POINT('Ctrl Pts',(98.6271369871057,-1.67787529767851,0.58310620540181));
#25403=CARTESIAN_POINT('Ctrl Pts',(98.6289489764837,-1.68660068306509,0.557315573032014));
#25404=CARTESIAN_POINT('Ctrl Pts',(98.6297908543013,-1.69050773137571,0.545349528412544));
#25405=CARTESIAN_POINT('Ctrl Pts',(98.6316788155087,-1.69894108765747,0.518559036508505));
#25406=CARTESIAN_POINT('Ctrl Pts',(98.6327269984785,-1.70340115010637,0.503714987754341));
#25407=CARTESIAN_POINT('Ctrl Pts',(98.6358142009334,-1.71588728261929,0.460094900941571));
#25408=CARTESIAN_POINT('Ctrl Pts',(98.6378701064034,-1.72338199963596,0.431173723486116));
#25409=CARTESIAN_POINT('Ctrl Pts',(98.6496118578181,-1.76158244788667,0.266797333653768));
#25410=CARTESIAN_POINT('Ctrl Pts',(98.6597745737697,-1.77704130590816,0.128315204723318));
#25411=CARTESIAN_POINT('Ctrl Pts',(98.6753244703899,-1.77578011922774,-0.0845794326828024));
#25412=CARTESIAN_POINT('Ctrl Pts',(98.6807007819412,-1.77071019573902,-0.158544002731478));
#25413=CARTESIAN_POINT('Ctrl Pts',(98.6871531795143,-1.75869201340312,-0.249777149980269));
#25414=CARTESIAN_POINT('Ctrl Pts',(98.6884004977045,-1.75607815253738,-0.26753655208544));
#25415=CARTESIAN_POINT('Ctrl Pts',(98.6902397272791,-1.75178042620321,-0.293950734562597));
#25416=CARTESIAN_POINT('Ctrl Pts',(98.6908419663048,-1.75030071227005,-0.302636945739618));
#25417=CARTESIAN_POINT('Ctrl Pts',(98.6918751046767,-1.74763548509284,-0.317608526650054));
#25418=CARTESIAN_POINT('Ctrl Pts',(98.6923076625196,-1.74648059900108,-0.323898882195918));
#25419=CARTESIAN_POINT('Ctrl Pts',(98.6933215921682,-1.74368131157944,-0.338695435045995));
#25420=CARTESIAN_POINT('Ctrl Pts',(98.6939013673405,-1.74200862743133,-0.347196002126398));
#25421=CARTESIAN_POINT('Ctrl Pts',(98.6956218738606,-1.7368312694828,-0.372527517922934));
#25422=CARTESIAN_POINT('Ctrl Pts',(98.6967529342113,-1.73314426243373,-0.389320728585039));
#25423=CARTESIAN_POINT('Ctrl Pts',(98.7067051547055,-1.69822512922198,-0.5380250326482));
#25424=CARTESIAN_POINT('Ctrl Pts',(98.714852794876,-1.65222733382778,-0.666029239217347));
#25425=CARTESIAN_POINT('Ctrl Pts',(98.7284898044332,-1.55410184525391,-0.864394764854116));
#25426=CARTESIAN_POINT('Ctrl Pts',(98.7338305891552,-1.51059069657303,-0.938362507798115));
#25427=CARTESIAN_POINT('Ctrl Pts',(98.7410347656329,-1.44716871950847,-1.03026244745366));
#25428=CARTESIAN_POINT('Ctrl Pts',(98.7427254591458,-1.43195733628363,-1.05130209171884));
#25429=CARTESIAN_POINT('Ctrl Pts',(98.7453899781658,-1.40752132847668,-1.08358613757846));
#25430=CARTESIAN_POINT('Ctrl Pts',(98.7463516137895,-1.39861008326424,-1.09506393491514));
#25431=CARTESIAN_POINT('Ctrl Pts',(98.7481573354621,-1.38171301983853,-1.11628484631996));
#25432=CARTESIAN_POINT('Ctrl Pts',(98.7489999779953,-1.373762382497,-1.12605489636957));
#25433=CARTESIAN_POINT('Ctrl Pts',(98.7508985234889,-1.35570729167018,-1.14776585877698));
#25434=CARTESIAN_POINT('Ctrl Pts',(98.7519566367536,-1.34554777082187,-1.15965938807568));
#25435=CARTESIAN_POINT('Ctrl Pts',(98.7546959680289,-1.31900612804613,-1.1899127268983));
#25436=CARTESIAN_POINT('Ctrl Pts',(98.7563864816377,-1.30239766536331,-1.20806857392049));
#25437=CARTESIAN_POINT('Ctrl Pts',(98.7654135191758,-1.21254712717535,-1.3022834953871));
#25438=CARTESIAN_POINT('Ctrl Pts',(98.7730184037613,-1.1330195401061,-1.37203244763905));
#25439=CARTESIAN_POINT('Ctrl Pts',(98.7867598095984,-0.981038595867624,
-1.48305753577234));
#25440=CARTESIAN_POINT('Ctrl Pts',(98.7928353713481,-0.910969693365428,
-1.52709902369894));
#25441=CARTESIAN_POINT('Ctrl Pts',(98.8007216822298,-0.814129666660991,
-1.57892217976014));
#25442=CARTESIAN_POINT('Ctrl Pts',(98.8026559734616,-0.789880305491776,
-1.59119188820044));
#25443=CARTESIAN_POINT('Ctrl Pts',(98.8059310273371,-0.747825033144203,
-1.61127255952482));
#25444=CARTESIAN_POINT('Ctrl Pts',(98.8072835985089,-0.730155243086849,
-1.61935633492277));
#25445=CARTESIAN_POINT('Ctrl Pts',(98.8092456467165,-0.704028887914428,
-1.63079428755314));
#25446=CARTESIAN_POINT('Ctrl Pts',(98.8098674678683,-0.695674192761286,
-1.6343757554316));
#25447=CARTESIAN_POINT('Ctrl Pts',(98.8109683782373,-0.680742530658057,
-1.64064137468307));
#25448=CARTESIAN_POINT('Ctrl Pts',(98.8114488954001,-0.674176531846912,
-1.64335039554523));
#25449=CARTESIAN_POINT('Ctrl Pts',(98.812516464792,-0.659479487156446,-1.64931123397924));
#25450=CARTESIAN_POINT('Ctrl Pts',(98.8131023006504,-0.651340458944043,
-1.65254239133418));
#25451=CARTESIAN_POINT('Ctrl Pts',(98.8148600603908,-0.626708875417907,
-1.66211076528193));
#25452=CARTESIAN_POINT('Ctrl Pts',(98.8160216812129,-0.610144793441377,
-1.66826244930331));
#25453=CARTESIAN_POINT('Ctrl Pts',(98.8238253475529,-0.497158532421888,
-1.70831601058425));
#25454=CARTESIAN_POINT('Ctrl Pts',(98.8300896204472,-0.398045422492196,
-1.73409210342019));
#25455=CARTESIAN_POINT('Ctrl Pts',(98.8414800174878,-0.215095904723764,
-1.76514654681028));
#25456=CARTESIAN_POINT('Ctrl Pts',(98.8465879756094,-0.13206097766988,-1.7732927947059));
#25457=CARTESIAN_POINT('Ctrl Pts',(98.8549759869495,0.000984312464261099,
-1.77694682007739));
#25458=CARTESIAN_POINT('Ctrl Pts',(98.8581585024249,0.0507655887931716,
-1.77622158975453));
#25459=CARTESIAN_POINT('Ctrl Pts',(98.86260976139,0.118880795877582,-1.77236347644932));
#25460=CARTESIAN_POINT('Ctrl Pts',(98.863822793402,0.137296022137774,-1.77103209920204));
#25461=CARTESIAN_POINT('Ctrl Pts',(98.8659048649879,0.168630359430165,-1.76827506414069));
#25462=CARTESIAN_POINT('Ctrl Pts',(98.8667693107381,0.181560933057691,-1.76699420283598));
#25463=CARTESIAN_POINT('Ctrl Pts',(98.8684237835398,0.206151542872894,-1.76428557099717));
#25464=CARTESIAN_POINT('Ctrl Pts',(98.8692129476589,0.217813788089008,-1.76288376725664));
#25465=CARTESIAN_POINT('Ctrl Pts',(98.871070182808,0.245097660709174,-1.75932937590262));
#25466=CARTESIAN_POINT('Ctrl Pts',(98.8721411209248,0.260706010851268,-1.75708425070233));
#25467=CARTESIAN_POINT('Ctrl Pts',(98.8759247362313,0.315401275171302,-1.74847200709364));
#25468=CARTESIAN_POINT('Ctrl Pts',(98.8786714290312,0.354300724598346,-1.74100628688364));
#25469=CARTESIAN_POINT('Ctrl Pts',(98.8904415437691,0.517555674101067,-1.70397611009358));
#25470=CARTESIAN_POINT('Ctrl Pts',(98.8998194007648,0.638766261996261,-1.66233793867587));
#25471=CARTESIAN_POINT('Ctrl Pts',(98.9142854474111,0.818207159846212,-1.57815155134061));
#25472=CARTESIAN_POINT('Ctrl Pts',(98.9193890960477,0.880144384773158,-1.54446529280055));
#25473=CARTESIAN_POINT('Ctrl Pts',(98.925556167253,0.954819678083148,-1.49789575488501));
#25474=CARTESIAN_POINT('Ctrl Pts',(98.9267756550597,0.96957930582316,-1.48838447251716));
#25475=CARTESIAN_POINT('Ctrl Pts',(98.9285822191231,0.991467682733885,-1.4738155233181));
#25476=CARTESIAN_POINT('Ctrl Pts',(98.929179115918,0.998703604855317,-1.46892187690465));
#25477=CARTESIAN_POINT('Ctrl Pts',(98.9302066664914,1.01117187945313,-1.46035487301818));
#25478=CARTESIAN_POINT('Ctrl Pts',(98.9306389185864,1.01642079469667,-1.45670645512857));
#25479=CARTESIAN_POINT('Ctrl Pts',(98.9316573092023,1.02879629237097,-1.44800502914916));
#25480=CARTESIAN_POINT('Ctrl Pts',(98.9322417906084,1.03590543215427,-1.44292769026064));
#25481=CARTESIAN_POINT('Ctrl Pts',(98.9339912151489,1.05719199545506,-1.42748644154262));
#25482=CARTESIAN_POINT('Ctrl Pts',(98.935145997999,1.07125394101419,-1.41696418693468));
#25483=CARTESIAN_POINT('Ctrl Pts',(98.9431672054606,1.1687850805004,-1.34170170256927));
#25484=CARTESIAN_POINT('Ctrl Pts',(98.9496286742871,1.24650015604602,-1.26982881640559));
#25485=CARTESIAN_POINT('Ctrl Pts',(98.9626802312856,1.38913449633555,-1.11212164058899));
#25486=CARTESIAN_POINT('Ctrl Pts',(98.9692496444194,1.45357344753965,-1.02646497876475));
#25487=CARTESIAN_POINT('Ctrl Pts',(98.9780866352389,1.52613272069163,-0.909357692274584));
#25488=CARTESIAN_POINT('Ctrl Pts',(98.9800833948425,1.54166862908891,-0.882762793228912));
#25489=CARTESIAN_POINT('Ctrl Pts',(98.9831213869077,1.56396580518879,-0.842208315683904));
#25490=CARTESIAN_POINT('Ctrl Pts',(98.9841440394403,1.57124893003603,-0.828541285207962));
#25491=CARTESIAN_POINT('Ctrl Pts',(98.9860094158675,1.58412594206036,-0.803596597524649));
#25492=CARTESIAN_POINT('Ctrl Pts',(98.9868499322321,1.58978046990137,-0.792351270174113));
#25493=CARTESIAN_POINT('Ctrl Pts',(98.9886778991063,1.6017566690981,-0.76788948001522));
#25494=CARTESIAN_POINT('Ctrl Pts',(98.9896667765806,1.60803525477435,-0.754653084190841));
#25495=CARTESIAN_POINT('Ctrl Pts',(98.992413899012,1.62492265813026,-0.717883508951439));
#25496=CARTESIAN_POINT('Ctrl Pts',(98.9941838603736,1.63518294028412,-0.694195222592844));
#25497=CARTESIAN_POINT('Ctrl Pts',(99.0051623376704,1.69502118552491,-0.547349992656807));
#25498=CARTESIAN_POINT('Ctrl Pts',(99.0148168437555,1.7311698234477,-0.41919876280801));
#25499=CARTESIAN_POINT('Ctrl Pts',(99.0292100396768,1.76310811693019,-0.224994899731161));
#25500=CARTESIAN_POINT('Ctrl Pts',(99.0338908562335,1.77007927957483,-0.161223912246889));
#25501=CARTESIAN_POINT('Ctrl Pts',(99.0396587094954,1.77449477108834,-0.0806659106480894));
#25502=CARTESIAN_POINT('Ctrl Pts',(99.0408364707886,1.77517010346589,-0.0641074739969688));
#25503=CARTESIAN_POINT('Ctrl Pts',(99.0420054636133,1.77561363841465,-0.0475422924970873));
#25504=CARTESIAN_POINT('Origin',(88.3562164250559,0.,0.));
#25505=CARTESIAN_POINT('',(99.938371422543,1.77561385491717,-0.0475342058543041));
#25506=CARTESIAN_POINT('',(99.7906385404719,1.77561363837197,-0.0475422940912401));
#25507=CARTESIAN_POINT('',(88.3562164250559,1.77561363837197,-0.0475422940912398));
#25508=CARTESIAN_POINT('Ctrl Pts',(99.9400048992461,1.77561095934877,-0.0476422453347091));
#25509=CARTESIAN_POINT('Ctrl Pts',(99.9392792521777,1.77531380150608,-0.0587172213027325));
#25510=CARTESIAN_POINT('Ctrl Pts',(99.9385505341127,1.77491303798314,-0.0697890155623971));
#25511=CARTESIAN_POINT('Ctrl Pts',(99.9369984403196,1.77384358538345,-0.0932584136990634));
#25512=CARTESIAN_POINT('Ctrl Pts',(99.9361742979604,1.77314844128254,-0.105654101208776));
#25513=CARTESIAN_POINT('Ctrl Pts',(99.9344996615558,1.7714802627955,-0.130700875105751));
#25514=CARTESIAN_POINT('Ctrl Pts',(99.9336490360991,1.77050150043317,-0.143350838123707));
#25515=CARTESIAN_POINT('Ctrl Pts',(99.9316524489825,1.76789937283275,-0.172866848806497));
#25516=CARTESIAN_POINT('Ctrl Pts',(99.9305032412245,1.76617004982319,-0.189722060810516));
#25517=CARTESIAN_POINT('Ctrl Pts',(99.9268197043723,1.75989646429347,-0.243306607235349));
#25518=CARTESIAN_POINT('Ctrl Pts',(99.9242575803557,1.75444560647524,-0.2799177247912));
#25519=CARTESIAN_POINT('Ctrl Pts',(99.9188907561589,1.74081754955114,-0.355218525302948));
#25520=CARTESIAN_POINT('Ctrl Pts',(99.9160828625299,1.73248391536634,-0.393859182768566));
#25521=CARTESIAN_POINT('Ctrl Pts',(99.9068863343339,1.70131242095907,-0.518120979208936));
#25522=CARTESIAN_POINT('Ctrl Pts',(99.9003871154567,1.6733577245273,-0.602316659261444));
#25523=CARTESIAN_POINT('Ctrl Pts',(99.8885033207208,1.61070886918589,-0.752442737875994));
#25524=CARTESIAN_POINT('Ctrl Pts',(99.8831240293653,1.57792324616843,-0.818970971649752));
#25525=CARTESIAN_POINT('Ctrl Pts',(99.8766607461606,1.53209825313043,-0.898924294433005));
#25526=CARTESIAN_POINT('Ctrl Pts',(99.875405976219,1.52288289342607,-0.914449397219466));
#25527=CARTESIAN_POINT('Ctrl Pts',(99.8735533210496,1.50877398085504,-0.937413630721445));
#25528=CARTESIAN_POINT('Ctrl Pts',(99.8729450395149,1.50405891905455,-0.944960325588245));
#25529=CARTESIAN_POINT('Ctrl Pts',(99.8719017297436,1.49582496966288,-0.957921401550772));
#25530=CARTESIAN_POINT('Ctrl Pts',(99.871465004197,1.49233303364727,-0.963352413437259));
#25531=CARTESIAN_POINT('Ctrl Pts',(99.8704414561022,1.48404183626071,-0.976094445538943));
#25532=CARTESIAN_POINT('Ctrl Pts',(99.8698562650296,1.47921810449177,-0.983389213818415));
#25533=CARTESIAN_POINT('Ctrl Pts',(99.8681121966172,1.46459806209791,-1.00514761448588));
#25534=CARTESIAN_POINT('Ctrl Pts',(99.8669633910738,1.45464174386018,-1.01950314568186));
#25535=CARTESIAN_POINT('Ctrl Pts',(99.8570888886245,1.36638987041332,-1.14282360682151));
#25536=CARTESIAN_POINT('Ctrl Pts',(99.8490232228396,1.2761820275638,-1.24275373112078));
#25537=CARTESIAN_POINT('Ctrl Pts',(99.8354415165225,1.11083491621752,-1.38872823491735));
#25538=CARTESIAN_POINT('Ctrl Pts',(99.8300658307838,1.04202826893568,-1.44107423976197));
#25539=CARTESIAN_POINT('Ctrl Pts',(99.822815779425,0.947837441630749,-1.50244757922321));
#25540=CARTESIAN_POINT('Ctrl Pts',(99.8211175361908,0.925671531266362,-1.51620468467212));
#25541=CARTESIAN_POINT('Ctrl Pts',(99.8184414050231,0.890646570793234,-1.53688831335412));
#25542=CARTESIAN_POINT('Ctrl Pts',(99.8174758928225,0.877990887495211,-1.54415316007862));
#25543=CARTESIAN_POINT('Ctrl Pts',(99.8156630005511,0.854202879532878,-1.55742140577891));
#25544=CARTESIAN_POINT('Ctrl Pts',(99.8148170862501,0.843093095928934,-1.56346346673544));
#25545=CARTESIAN_POINT('Ctrl Pts',(99.8129112722668,0.818047393114282,-1.57674000765449));
#25546=CARTESIAN_POINT('Ctrl Pts',(99.8118491340533,0.80407831081921,-1.58390928760646));
#25547=CARTESIAN_POINT('Ctrl Pts',(99.8090994969535,0.767899129692909,-1.60187539864835));
#25548=CARTESIAN_POINT('Ctrl Pts',(99.8074025790595,0.745556248085736,-1.61239562138282));
#25549=CARTESIAN_POINT('Ctrl Pts',(99.7983819927947,0.626753416003302,-1.66533710957251));
#25550=CARTESIAN_POINT('Ctrl Pts',(99.790789515764,0.526894156329278,-1.69957157426181));
#25551=CARTESIAN_POINT('Ctrl Pts',(99.7770031165378,0.343660052257937,-1.74468083967509));
#25552=CARTESIAN_POINT('Ctrl Pts',(99.770869800802,0.261409366537865,-1.75888585157346));
#25553=CARTESIAN_POINT('Ctrl Pts',(99.7629159480555,0.151270746352097,-1.77000796365344));
#25554=CARTESIAN_POINT('Ctrl Pts',(99.7609691631254,0.124017058489385,-1.77212611326942));
#25555=CARTESIAN_POINT('Ctrl Pts',(99.7576745026277,0.0772252176373467,
-1.77467790295851));
#25556=CARTESIAN_POINT('Ctrl Pts',(99.7563145813094,0.057709255188337,-1.7754197008849));
#25557=CARTESIAN_POINT('Ctrl Pts',(99.7543430091102,0.0290627801484523,
-1.77603565654665));
#25558=CARTESIAN_POINT('Ctrl Pts',(99.7537187894799,0.0199398800334438,
-1.77616150981563));
#25559=CARTESIAN_POINT('Ctrl Pts',(99.7526123540901,0.00366713514776551,
-1.77626060169673));
#25560=CARTESIAN_POINT('Ctrl Pts',(99.7521287122019,-0.00348198047841314,
-1.7762609755629));
#25561=CARTESIAN_POINT('Ctrl Pts',(99.7510521069026,-0.0194762158373868,
-1.77616524410506));
#25562=CARTESIAN_POINT('Ctrl Pts',(99.7504604057516,-0.0283208211096542,
-1.77604623723244));
#25563=CARTESIAN_POINT('Ctrl Pts',(99.7486847258366,-0.0550129008027708,
-1.7754876377026));
#25564=CARTESIAN_POINT('Ctrl Pts',(99.7475112590055,-0.0728555946040405,
-1.77484503353384));
#25565=CARTESIAN_POINT('Ctrl Pts',(99.7398221239447,-0.190856629995937,
-1.76881262694266));
#25566=CARTESIAN_POINT('Ctrl Pts',(99.7336685694406,-0.290426464850753,
-1.75521564326854));
#25567=CARTESIAN_POINT('Ctrl Pts',(99.7248323280064,-0.430893613010248,
-1.72374525363767));
#25568=CARTESIAN_POINT('Ctrl Pts',(99.7221578903596,-0.473094878815755,
-1.71264361633276));
#25569=CARTESIAN_POINT('Ctrl Pts',(99.7153225145289,-0.578965032774141,
-1.68058089631236));
#25570=CARTESIAN_POINT('Ctrl Pts',(99.7111369461174,-0.641930697904599,
-1.6575513342473));
#25571=CARTESIAN_POINT('Ctrl Pts',(99.7048149888961,-0.732513790773486,
-1.61848386212147));
#25572=CARTESIAN_POINT('Ctrl Pts',(99.7027636764108,-0.761243948389654,
-1.60517099380572));
#25573=CARTESIAN_POINT('Ctrl Pts',(99.6996521933884,-0.803719061091138,
-1.58409220598707));
#25574=CARTESIAN_POINT('Ctrl Pts',(99.6986117595525,-0.817742190328487,
-1.57689889647653));
#25575=CARTESIAN_POINT('Ctrl Pts',(99.6967181221554,-0.842928011231842,
-1.56355327239801));
#25576=CARTESIAN_POINT('Ctrl Pts',(99.6958672457838,-0.854123844266056,
-1.55746554114823));
#25577=CARTESIAN_POINT('Ctrl Pts',(99.69402118773,-0.878147613338086,-1.54406568295718));
#25578=CARTESIAN_POINT('Ctrl Pts',(99.6930245993296,-0.890951739418545,
-1.5367130633913));
#25579=CARTESIAN_POINT('Ctrl Pts',(99.6902667353676,-0.925923183817079,
-1.51604713323828));
#25580=CARTESIAN_POINT('Ctrl Pts',(99.6884938009734,-0.947893001584265,
-1.50240852890187));
#25581=CARTESIAN_POINT('Ctrl Pts',(99.6767724349312,-1.08975192908441,-1.40999395846063));
#25582=CARTESIAN_POINT('Ctrl Pts',(99.6662955626293,-1.19999981145682,-1.31743224038946));
#25583=CARTESIAN_POINT('Ctrl Pts',(99.6503314610838,-1.34924967021319,-1.15769038922376));
#25584=CARTESIAN_POINT('Ctrl Pts',(99.6448692042926,-1.39706286175475,-1.09951770787243));
#25585=CARTESIAN_POINT('Ctrl Pts',(99.6383198288909,-1.45166331899783,-1.02375163381629));
#25586=CARTESIAN_POINT('Ctrl Pts',(99.6370577693318,-1.46205375954034,-1.00885710946254));
#25587=CARTESIAN_POINT('Ctrl Pts',(99.6351965077656,-1.4772052608326,-0.986411805413159));
#25588=CARTESIAN_POINT('Ctrl Pts',(99.6345867946377,-1.48214045131977,-0.978980757547719));
#25589=CARTESIAN_POINT('Ctrl Pts',(99.6335408124788,-1.49056155263733,-0.966091226365382));
#25590=CARTESIAN_POINT('Ctrl Pts',(99.6331028493312,-1.49407382481972,-0.960650513844036));
#25591=CARTESIAN_POINT('Ctrl Pts',(99.6320752740193,-1.50228194358447,-0.947781748736228));
#25592=CARTESIAN_POINT('Ctrl Pts',(99.6314873073003,-1.5069525203552,-0.940337913113716));
#25593=CARTESIAN_POINT('Ctrl Pts',(99.6297726079399,-1.52048907246235,-0.918403832452889));
#25594=CARTESIAN_POINT('Ctrl Pts',(99.6286551172428,-1.52920293552013,-0.903820254677063));
#25595=CARTESIAN_POINT('Ctrl Pts',(99.6187106805063,-1.60560059805604,-0.771691766231914));
#25596=CARTESIAN_POINT('Ctrl Pts',(99.6105574799591,-1.65983126352376,-0.646863368455838));
#25597=CARTESIAN_POINT('Ctrl Pts',(99.5983844292871,-1.71732902175815,-0.457897146413347));
#25598=CARTESIAN_POINT('Ctrl Pts',(99.5945429649507,-1.7322284499121,-0.397834817794887));
#25599=CARTESIAN_POINT('Ctrl Pts',(99.58799479525,-1.75180934750379,-0.296540702316916));
#25600=CARTESIAN_POINT('Ctrl Pts',(99.5853367672581,-1.75823454459147,-0.255701484365897));
#25601=CARTESIAN_POINT('Ctrl Pts',(99.5814973861227,-1.7653311808215,-0.197414115403766));
#25602=CARTESIAN_POINT('Ctrl Pts',(99.5803526893854,-1.76717934810694,-0.180121145564705));
#25603=CARTESIAN_POINT('Ctrl Pts',(99.5783439666791,-1.76995701254263,-0.149943454102504));
#25604=CARTESIAN_POINT('Ctrl Pts',(99.577483578208,-1.77100044245696,-0.137070359363327));
#25605=CARTESIAN_POINT('Ctrl Pts',(99.5756919457403,-1.7728710226764,-0.110380939572005));
#25606=CARTESIAN_POINT('Ctrl Pts',(99.5747601053092,-1.77367724657241,-0.0965640770739489));
#25607=CARTESIAN_POINT('Ctrl Pts',(99.5723208687671,-1.77535556627284,-0.0605730682739813));
#25608=CARTESIAN_POINT('Ctrl Pts',(99.5708056613789,-1.77597370635523,-0.0383900994893181));
#25609=CARTESIAN_POINT('Ctrl Pts',(99.5633995410787,-1.77695471708159,0.0691536612728943));
#25610=CARTESIAN_POINT('Ctrl Pts',(99.5573340018839,-1.77157955834121,0.154441982225163));
#25611=CARTESIAN_POINT('Ctrl Pts',(99.5434710263297,-1.74582305589433,0.344121463576641));
#25612=CARTESIAN_POINT('Ctrl Pts',(99.5356332822249,-1.72216148013362,0.447746490714757));
#25613=CARTESIAN_POINT('Ctrl Pts',(99.5257745371451,-1.6799104182754,0.577847852038138));
#25614=CARTESIAN_POINT('Ctrl Pts',(99.5235801883268,-1.66966848831537,0.606806810991485));
#25615=CARTESIAN_POINT('Ctrl Pts',(99.5199159153223,-1.65106312672038,0.655368524575739));
#25616=CARTESIAN_POINT('Ctrl Pts',(99.5184305741234,-1.64308874987426,0.675112443245771));
#25617=CARTESIAN_POINT('Ctrl Pts',(99.5163113338566,-1.63105426898313,0.703431482326731));
#25618=CARTESIAN_POINT('Ctrl Pts',(99.5156623728187,-1.62727781093949,0.71212415697693));
#25619=CARTESIAN_POINT('Ctrl Pts',(99.5145282781634,-1.62051380663837,0.727358766740251));
#25620=CARTESIAN_POINT('Ctrl Pts',(99.5140414411001,-1.61755586197693,0.733913355206157));
#25621=CARTESIAN_POINT('Ctrl Pts',(99.5129767898867,-1.61096676102347,0.748280946912124));
#25622=CARTESIAN_POINT('Ctrl Pts',(99.5124000171557,-1.60731848528246,0.756085693070234));
#25623=CARTESIAN_POINT('Ctrl Pts',(99.5107471456957,-1.5966410717615,0.778501265610848));
#25624=CARTESIAN_POINT('Ctrl Pts',(99.5096793495866,-1.58946828092328,0.793043228406025));
#25625=CARTESIAN_POINT('Ctrl Pts',(99.5008415912529,-1.52789425438043,0.913684502815119));
#25626=CARTESIAN_POINT('Ctrl Pts',(99.493601590606,-1.46312834122856,1.01417143867414));
#25627=CARTESIAN_POINT('Ctrl Pts',(99.4804804603201,-1.32992641536686,1.18121472859065));
#25628=CARTESIAN_POINT('Ctrl Pts',(99.4746531293541,-1.26529930309067,1.25019504500519));
#25629=CARTESIAN_POINT('Ctrl Pts',(99.4665952006454,-1.17233060216966,1.33479834431371));
#25630=CARTESIAN_POINT('Ctrl Pts',(99.464564864965,-1.1486060131395,1.35526738894227));
#25631=CARTESIAN_POINT('Ctrl Pts',(99.4614804359575,-1.11221992440914,1.38501861360285));
#25632=CARTESIAN_POINT('Ctrl Pts',(99.4604456449017,-1.09995573949492,1.39477850038196));
#25633=CARTESIAN_POINT('Ctrl Pts',(99.4585600797156,-1.07751736270954,1.41215504566552));
#25634=CARTESIAN_POINT('Ctrl Pts',(99.4577115898142,-1.06738742833346,1.41982731461435));
#25635=CARTESIAN_POINT('Ctrl Pts',(99.4558682938061,-1.04531622381875,1.43617404014555));
#25636=CARTESIAN_POINT('Ctrl Pts',(99.4548720571789,-1.03334748611272,1.44480961768282));
#25637=CARTESIAN_POINT('Ctrl Pts',(99.452109095913,-1.00005320888311,1.46820648139115));
#25638=CARTESIAN_POINT('Ctrl Pts',(99.4503305675742,-0.978510575681864,
1.48265087663836));
#25639=CARTESIAN_POINT('Ctrl Pts',(99.4393650406622,-0.845083703505877,
1.56793931940031));
#25640=CARTESIAN_POINT('Ctrl Pts',(99.4297346032892,-0.725899861980511,
1.62654768766169));
#25641=CARTESIAN_POINT('Ctrl Pts',(99.4132261851446,-0.513513059204109,
1.70296219279321));
#25642=CARTESIAN_POINT('Ctrl Pts',(99.406412628982,-0.423323860294552,1.72759267593499));
#25643=CARTESIAN_POINT('Ctrl Pts',(99.3989092240858,-0.317537418872479,
1.7476953949356));
#25644=CARTESIAN_POINT('Ctrl Pts',(99.3979188592608,-0.303434005996591,
1.75019914373216));
#25645=CARTESIAN_POINT('Ctrl Pts',(99.3963811588102,-0.281291185585047,
1.75385439581656));
#25646=CARTESIAN_POINT('Ctrl Pts',(99.395827783108,-0.273271899624891,1.75512177592375));
#25647=CARTESIAN_POINT('Ctrl Pts',(99.3947828513343,-0.258027197697644,
1.75742405182669));
#25648=CARTESIAN_POINT('Ctrl Pts',(99.3942907632141,-0.250803755068399,
1.75846945123871));
#25649=CARTESIAN_POINT('Ctrl Pts',(99.3931074145119,-0.233330856136563,
1.76088832852753));
#25650=CARTESIAN_POINT('Ctrl Pts',(99.3924186187754,-0.223075277598957,
1.76221690702849));
#25651=CARTESIAN_POINT('Ctrl Pts',(99.3900901545508,-0.188141699620423,
1.76643258260177));
#25652=CARTESIAN_POINT('Ctrl Pts',(99.3884720624082,-0.163413785774393,
1.76889158833672));
#25653=CARTESIAN_POINT('Ctrl Pts',(99.3787860734461,-0.0132833053826002,
1.78064552423622));
#25654=CARTESIAN_POINT('Ctrl Pts',(99.3712145071567,0.112775518964679,1.77712229812572));
#25655=CARTESIAN_POINT('Ctrl Pts',(99.3582908978089,0.320502485080232,1.74910580232864));
#25656=CARTESIAN_POINT('Ctrl Pts',(99.3530614820441,0.402682228437745,1.73203281494645));
#25657=CARTESIAN_POINT('Ctrl Pts',(99.3459862975025,0.50818242865288,1.70219886459313));
#25658=CARTESIAN_POINT('Ctrl Pts',(99.3443049547342,0.532863873231661,1.69463457343424));
#25659=CARTESIAN_POINT('Ctrl Pts',(99.3416457711371,0.57122700964473,1.68195622162478));
#25660=CARTESIAN_POINT('Ctrl Pts',(99.3406798730468,0.585025949542344,1.67720650040071));
#25661=CARTESIAN_POINT('Ctrl Pts',(99.3388603405357,0.610755940497993,1.66799384708985));
#25662=CARTESIAN_POINT('Ctrl Pts',(99.338008104977,0.622700613752867,1.66357152651223));
#25663=CARTESIAN_POINT('Ctrl Pts',(99.3360798469588,0.649480136139083,1.65332802326466));
#25664=CARTESIAN_POINT('Ctrl Pts',(99.3350014667269,0.664286113416507,1.64743495482028));
#25665=CARTESIAN_POINT('Ctrl Pts',(99.3321915025723,0.70241576887303,1.63166102944136));
#25666=CARTESIAN_POINT('Ctrl Pts',(99.3304499398288,0.725610252672839,1.62147934731486));
#25667=CARTESIAN_POINT('Ctrl Pts',(99.3188781813886,0.876810879562657,1.55121296927954));
#25668=CARTESIAN_POINT('Ctrl Pts',(99.3085394090597,0.997448841115302,1.47652997338205));
#25669=CARTESIAN_POINT('Ctrl Pts',(99.292757123101,1.16632940484223,1.34176053312714));
#25670=CARTESIAN_POINT('Ctrl Pts',(99.2873316344231,1.22173194500975,1.29151801145696));
#25671=CARTESIAN_POINT('Ctrl Pts',(99.2808222364033,1.28641841376054,1.22495674981306));
#25672=CARTESIAN_POINT('Ctrl Pts',(99.279564782693,1.29882885688778,1.21179001394723));
#25673=CARTESIAN_POINT('Ctrl Pts',(99.2777099214663,1.31703667078401,1.19187145132884));
#25674=CARTESIAN_POINT('Ctrl Pts',(99.2771020453949,1.32298758720841,1.18526241875934));
#25675=CARTESIAN_POINT('Ctrl Pts',(99.2760587791879,1.33317695828544,1.17377383924956));
#25676=CARTESIAN_POINT('Ctrl Pts',(99.2756217056807,1.33743868534919,1.16891556343645));
#25677=CARTESIAN_POINT('Ctrl Pts',(99.2745957466579,1.34742539695441,1.1574048059943));
#25678=CARTESIAN_POINT('Ctrl Pts',(99.2740085084895,1.35312770827142,1.1507330266272));
#25679=CARTESIAN_POINT('Ctrl Pts',(99.2722603634668,1.37005164552685,1.13063203699189));
#25680=CARTESIAN_POINT('Ctrl Pts',(99.2711094941957,1.38112487471722,1.11707853417323));
#25681=CARTESIAN_POINT('Ctrl Pts',(99.2612388272418,1.47528352954298,0.998288507725664));
#25682=CARTESIAN_POINT('Ctrl Pts',(99.2531741563852,1.54641737843456,0.884106868278432));
#25683=CARTESIAN_POINT('Ctrl Pts',(99.2395914388576,1.64112501813017,0.685004458460632));
#25684=CARTESIAN_POINT('Ctrl Pts',(99.2342128648273,1.67248107709777,0.604422902659847));
#25685=CARTESIAN_POINT('Ctrl Pts',(99.2269561200872,1.70553528107832,0.496887753225648));
#25686=CARTESIAN_POINT('Ctrl Pts',(99.2252531992854,1.71266596037846,0.47172367728203));
#25687=CARTESIAN_POINT('Ctrl Pts',(99.2225677244021,1.72292285971994,0.432221963871046));
#25688=CARTESIAN_POINT('Ctrl Pts',(99.2215975234154,1.72643157187855,0.417986856902056));
#25689=CARTESIAN_POINT('Ctrl Pts',(99.2197744587135,1.73265609629284,0.391316851957801));
#25690=CARTESIAN_POINT('Ctrl Pts',(99.2189230534486,1.73541526266783,0.378892964028254));
#25691=CARTESIAN_POINT('Ctrl Pts',(99.2170027972605,1.74130663515942,0.350949990746207));
#25692=CARTESIAN_POINT('Ctrl Pts',(99.2159316676685,1.74436530237799,0.335416691834679));
#25693=CARTESIAN_POINT('Ctrl Pts',(99.2126659819314,1.75300257111312,0.288233924499014));
#25694=CARTESIAN_POINT('Ctrl Pts',(99.2104511826106,1.75793000450438,0.256473537490275));
#25695=CARTESIAN_POINT('Ctrl Pts',(99.2018629622776,1.77350429536551,0.13429209840756));
#25696=CARTESIAN_POINT('Ctrl Pts',(99.1953165639767,1.77804619474441,0.0433090279489397));
#25697=CARTESIAN_POINT('Ctrl Pts',(99.1886897733872,1.77561363837197,-0.0475422940912343));
#25698=CARTESIAN_POINT('Ctrl Pts',(99.0420054636133,1.77561363841465,-0.0475422924970873));
#25699=CARTESIAN_POINT('Ctrl Pts',(99.0432892873456,1.77610074208309,-0.029349902698944));
#25700=CARTESIAN_POINT('Ctrl Pts',(99.0445625357543,1.77630827248011,-0.0111493778985186));
#25701=CARTESIAN_POINT('Ctrl Pts',(99.0466052615637,1.77619111743689,0.0183558676580814));
#25702=CARTESIAN_POINT('Ctrl Pts',(99.0473826964922,1.77603834619032,0.0296586110785028));
#25703=CARTESIAN_POINT('Ctrl Pts',(99.0486612332802,1.77560649672732,0.0483812222678931));
#25704=CARTESIAN_POINT('Ctrl Pts',(99.0491655764023,1.77538877824435,0.0558020332029134));
#25705=CARTESIAN_POINT('Ctrl Pts',(99.0501851804467,1.77485174892134,0.0708806680593242));
#25706=CARTESIAN_POINT('Ctrl Pts',(99.0507002718848,1.77452939136981,0.0785381724348064));
#25707=CARTESIAN_POINT('Ctrl Pts',(99.0520437423076,1.77355436430919,0.0986075615288776));
#25708=CARTESIAN_POINT('Ctrl Pts',(99.0528677924276,1.77282095743971,0.111015354235097));
#25709=CARTESIAN_POINT('Ctrl Pts',(99.0564801458365,1.76900657735169,0.165781198002898));
#25710=CARTESIAN_POINT('Ctrl Pts',(99.0592013510977,1.76453706022991,0.208031907885738));
#25711=CARTESIAN_POINT('Ctrl Pts',(99.0679776109073,1.74494311017726,0.345813207589858));
#25712=CARTESIAN_POINT('Ctrl Pts',(99.0738465368231,1.72353509891961,0.440275213959686));
#25713=CARTESIAN_POINT('Ctrl Pts',(99.0853080267608,1.66770723420564,0.617922978705789));
#25714=CARTESIAN_POINT('Ctrl Pts',(99.0908726661741,1.63445813853118,0.701156341888515));
#25715=CARTESIAN_POINT('Ctrl Pts',(99.0983495247431,1.5834370898929,0.805289649538533));
#25716=CARTESIAN_POINT('Ctrl Pts',(99.1000721935234,1.57126390996472,0.82879071172082));
#25717=CARTESIAN_POINT('Ctrl Pts',(99.1027758685017,1.55155137827189,0.864850584095201));
#25718=CARTESIAN_POINT('Ctrl Pts',(99.1037440752267,1.54437375702883,0.877603492064699));
#25719=CARTESIAN_POINT('Ctrl Pts',(99.1055557270017,1.53073033691304,0.901158786466298));
#25720=CARTESIAN_POINT('Ctrl Pts',(99.1063976436872,1.52430564233796,0.911984000642247));
#25721=CARTESIAN_POINT('Ctrl Pts',(99.108286158266,1.5097109560891,0.935990039442954));
#25722=CARTESIAN_POINT('Ctrl Pts',(99.109334861521,1.50148240390291,0.949133862529524));
#25723=CARTESIAN_POINT('Ctrl Pts',(99.1120325435817,1.48000646096914,0.982460027120919));
#25724=CARTESIAN_POINT('Ctrl Pts',(99.1136903450453,1.46651815381288,1.00248253565721));
#25725=CARTESIAN_POINT('Ctrl Pts',(99.1240115026733,1.3807985323342,1.12429410084689));
#25726=CARTESIAN_POINT('Ctrl Pts',(99.133064532903,1.29842427558394,1.21849329315012));
#25727=CARTESIAN_POINT('Ctrl Pts',(99.1472344620872,1.15626794806983,1.35013572344426));
#25728=CARTESIAN_POINT('Ctrl Pts',(99.1522814701665,1.10296789944966,1.39401749244203));
#25729=CARTESIAN_POINT('Ctrl Pts',(99.1598186615983,1.01792406157426,1.45609504200487));
#25730=CARTESIAN_POINT('Ctrl Pts',(99.1623852570002,0.987947857069246,1.47659798969468));
#25731=CARTESIAN_POINT('Ctrl Pts',(99.1656946796753,0.947699840814268,1.50235170792423));
#25732=CARTESIAN_POINT('Ctrl Pts',(99.1664839158295,0.937977749651262,1.50844071851244));
#25733=CARTESIAN_POINT('Ctrl Pts',(99.1677765901112,0.921837954093644,1.5183327952488));
#25734=CARTESIAN_POINT('Ctrl Pts',(99.168283410278,0.915454204860696,1.52219029561664));
#25735=CARTESIAN_POINT('Ctrl Pts',(99.1693026778979,0.902498735611143,1.52990789784766));
#25736=CARTESIAN_POINT('Ctrl Pts',(99.1698150078892,0.895926124456394,1.53376612582198));
#25737=CARTESIAN_POINT('Ctrl Pts',(99.1711426271564,0.878742626091827,1.54370496389767));
#25738=CARTESIAN_POINT('Ctrl Pts',(99.1719537735807,0.868093205618535,1.54971862785812));
#25739=CARTESIAN_POINT('Ctrl Pts',(99.1754080840351,0.822139438171575,1.57504607861606));
#25740=CARTESIAN_POINT('Ctrl Pts',(99.1779912546023,0.78624375102347,1.59326856488484));
#25741=CARTESIAN_POINT('Ctrl Pts',(99.1867456263915,0.660655153695733,1.65174427654853));
#25742=CARTESIAN_POINT('Ctrl Pts',(99.192710994448,0.568257969306344,1.68576682996564));
#25743=CARTESIAN_POINT('Ctrl Pts',(99.2043192225569,0.386446847465715,1.73605408299114));
#25744=CARTESIAN_POINT('Ctrl Pts',(99.2099325103568,0.297677575490778,1.75345668900032));
#25745=CARTESIAN_POINT('Ctrl Pts',(99.2174686074734,0.181586577711848,1.7671435858428));
#25746=CARTESIAN_POINT('Ctrl Pts',(99.2191980960664,0.155131972944316,1.76966213981009));
#25747=CARTESIAN_POINT('Ctrl Pts',(99.2219101409578,0.114014316283613,1.77264762395241));
#25748=CARTESIAN_POINT('Ctrl Pts',(99.2228797670406,0.0993845283088616,
1.77352799721832));
#25749=CARTESIAN_POINT('Ctrl Pts',(99.2246927561435,0.072173050022952,1.77482775223062));
#25750=CARTESIAN_POINT('Ctrl Pts',(99.2255345730323,0.0595944783970281,
1.77529461873417));
#25751=CARTESIAN_POINT('Ctrl Pts',(99.2274211510333,0.0315374759813947,
1.77603746795361));
#25752=CARTESIAN_POINT('Ctrl Pts',(99.2284679963782,0.0160584200929307,
1.77624485941758));
#25753=CARTESIAN_POINT('Ctrl Pts',(99.2311574066812,-0.0234691334653549,
1.77625774520556));
#25754=CARTESIAN_POINT('Ctrl Pts',(99.2328087009123,-0.0475139116236059,
1.77577721218532));
#25755=CARTESIAN_POINT('Ctrl Pts',(99.2450917824138,-0.224655602862794,
1.76863683066527));
#25756=CARTESIAN_POINT('Ctrl Pts',(99.2563388094861,-0.376304968175417,
1.74267701529871));
#25757=CARTESIAN_POINT('Ctrl Pts',(99.2711077324227,-0.569878370148193,
1.68307431336017));
#25758=CARTESIAN_POINT('Ctrl Pts',(99.2746851855186,-0.616430079077429,
1.66658784751913));
#25759=CARTESIAN_POINT('Ctrl Pts',(99.2802968719213,-0.689626156049868,
1.63717778371984));
#25760=CARTESIAN_POINT('Ctrl Pts',(99.2823722837504,-0.716738624041437,
1.62549110103071));
#25761=CARTESIAN_POINT('Ctrl Pts',(99.2851499516887,-0.753234740449387,
1.6086687768326));
#25762=CARTESIAN_POINT('Ctrl Pts',(99.285882505262,-0.762880381969297,1.60411699849026));
#25763=CARTESIAN_POINT('Ctrl Pts',(99.2871077919186,-0.779058113458006,
1.59630379509152));
#25764=CARTESIAN_POINT('Ctrl Pts',(99.2876032382343,-0.785612063855842,
1.59308852338859));
#25765=CARTESIAN_POINT('Ctrl Pts',(99.2886269539362,-0.799183429840687,
1.58632648709598));
#25766=CARTESIAN_POINT('Ctrl Pts',(99.2891548325884,-0.806197392030392,
1.58277340427916));
#25767=CARTESIAN_POINT('Ctrl Pts',(99.2905711823503,-0.825051300539528,
1.57306467766297));
#25768=CARTESIAN_POINT('Ctrl Pts',(99.2914544336315,-0.836846123196716,
1.56682185368301));
#25769=CARTESIAN_POINT('Ctrl Pts',(99.295917550194,-0.896560469117792,1.53434922623438));
#25770=CARTESIAN_POINT('Ctrl Pts',(99.2993848921658,-0.943326691737096,
1.50604920374993));
#25771=CARTESIAN_POINT('Ctrl Pts',(99.3096805000545,-1.0802687265442,1.41429409752211));
#25772=CARTESIAN_POINT('Ctrl Pts',(99.3163307999408,-1.16591373935445,1.34456500967248));
#25773=CARTESIAN_POINT('Ctrl Pts',(99.3276975514788,-1.29649112588474,1.21633672839006));
#25774=CARTESIAN_POINT('Ctrl Pts',(99.3322896698326,-1.34524478937329,1.16218712138409));
#25775=CARTESIAN_POINT('Ctrl Pts',(99.3383701899041,-1.4034568537298,1.08894636090368));
#25776=CARTESIAN_POINT('Ctrl Pts',(99.3397303704078,-1.41609155920959,1.07246443014137));
#25777=CARTESIAN_POINT('Ctrl Pts',(99.3419900545939,-1.43642708980782,1.04495077513096));
#25778=CARTESIAN_POINT('Ctrl Pts',(99.3428829094727,-1.44429693340484,1.03404606185917));
#25779=CARTESIAN_POINT('Ctrl Pts',(99.3446317015374,-1.45938570938459,1.01263023048757));
#25780=CARTESIAN_POINT('Ctrl Pts',(99.3454871010975,-1.46661678643711,1.00212864418156));
#25781=CARTESIAN_POINT('Ctrl Pts',(99.3475482328559,-1.48367972825955,0.976768118861398));
#25782=CARTESIAN_POINT('Ctrl Pts',(99.348757980751,-1.49340213502523,0.961837572949676));
#25783=CARTESIAN_POINT('Ctrl Pts',(99.3528383497562,-1.52521093968469,0.911344101748684));
#25784=CARTESIAN_POINT('Ctrl Pts',(99.3557458916567,-1.546263014484,0.875149511328884));
#25785=CARTESIAN_POINT('Ctrl Pts',(99.3693812403015,-1.63760254700222,0.704508843364687));
#25786=CARTESIAN_POINT('Ctrl Pts',(99.3806267310964,-1.69175624209207,0.562159362751232));
#25787=CARTESIAN_POINT('Ctrl Pts',(99.3953467076809,-1.73926485341889,0.364292562724473));
#25788=CARTESIAN_POINT('Ctrl Pts',(99.3990499103184,-1.74915637591595,0.313375705525583));
#25789=CARTESIAN_POINT('Ctrl Pts',(99.4035403303765,-1.75869429079464,0.249443505924488));
#25790=CARTESIAN_POINT('Ctrl Pts',(99.404422573216,-1.76044502314089,0.236772074930093));
#25791=CARTESIAN_POINT('Ctrl Pts',(99.4058272285281,-1.76303551462548,0.216401895961216));
#25792=CARTESIAN_POINT('Ctrl Pts',(99.4063541936045,-1.76396204485191,0.208714916883869));
#25793=CARTESIAN_POINT('Ctrl Pts',(99.4073711786707,-1.76566233481554,0.193787507265233));
#25794=CARTESIAN_POINT('Ctrl Pts',(99.4078614863327,-1.76644188193674,0.186548006820078));
#25795=CARTESIAN_POINT('Ctrl Pts',(99.4090833226112,-1.76828260252271,0.168406290473624));
#25796=CARTESIAN_POINT('Ctrl Pts',(99.4098117893353,-1.76928751227249,0.157498429045854));
#25797=CARTESIAN_POINT('Ctrl Pts',(99.4124814728353,-1.77262301164909,0.117217305697917));
#25798=CARTESIAN_POINT('Ctrl Pts',(99.4143914517961,-1.77432367816289,0.087794992966839));
#25799=CARTESIAN_POINT('Ctrl Pts',(99.4195064829357,-1.7769513627159,0.007837107781896));
#25800=CARTESIAN_POINT('Ctrl Pts',(99.4226592852629,-1.77645526996791,-0.0427192022554856));
#25801=CARTESIAN_POINT('Ctrl Pts',(99.4333140768053,-1.76741283978097,-0.214837798277852));
#25802=CARTESIAN_POINT('Ctrl Pts',(99.4406721279363,-1.74852552867487,-0.335501403474995));
#25803=CARTESIAN_POINT('Ctrl Pts',(99.4512606222229,-1.70575649953419,-0.497548848671729));
#25804=CARTESIAN_POINT('Ctrl Pts',(99.4541933857084,-1.69236706164545,-0.541343952642791));
#25805=CARTESIAN_POINT('Ctrl Pts',(99.4583827222333,-1.67123666944194,-0.60197317309261));
#25806=CARTESIAN_POINT('Ctrl Pts',(99.4595936261781,-1.66490119705217,-0.619279959715436));
#25807=CARTESIAN_POINT('Ctrl Pts',(99.4616646285539,-1.6536901188701,-0.648489320709872));
#25808=CARTESIAN_POINT('Ctrl Pts',(99.4625200751906,-1.64895234383836,-0.660443458012944));
#25809=CARTESIAN_POINT('Ctrl Pts',(99.4642681155468,-1.63905775038948,-0.68463871422407));
#25810=CARTESIAN_POINT('Ctrl Pts',(99.4651609475684,-1.63389258630172,-0.696875511043717));
#25811=CARTESIAN_POINT('Ctrl Pts',(99.4674065458348,-1.62062764647262,-0.727343135443157));
#25812=CARTESIAN_POINT('Ctrl Pts',(99.4687650640643,-1.61235724381205,-0.745497194371389));
#25813=CARTESIAN_POINT('Ctrl Pts',(99.4744715500483,-1.5766155052103,-0.820574385555406));
#25814=CARTESIAN_POINT('Ctrl Pts',(99.4789118357835,-1.54642456437316,-0.876143927188428));
#25815=CARTESIAN_POINT('Ctrl Pts',(99.4932409811137,-1.44156772339623,-1.04677536934854));
#25816=CARTESIAN_POINT('Ctrl Pts',(99.5034209365941,-1.35652492448684,-1.15485551100838));
#25817=CARTESIAN_POINT('Ctrl Pts',(99.5162287698012,-1.23093010844199,-1.2812357384225));
#25818=CARTESIAN_POINT('Ctrl Pts',(99.5191467371018,-1.20094684118452,-1.30938199797962));
#25819=CARTESIAN_POINT('Ctrl Pts',(99.5228541013217,-1.16074990438188,-1.34457251024279));
#25820=CARTESIAN_POINT('Ctrl Pts',(99.523702366848,-1.151404098962,-1.35258426654439));
#25821=CARTESIAN_POINT('Ctrl Pts',(99.5250661439311,-1.13612464304131,-1.36540953859781));
#25822=CARTESIAN_POINT('Ctrl Pts',(99.525585765161,-1.1302420886398,-1.37028290483263));
#25823=CARTESIAN_POINT('Ctrl Pts',(99.526606500248,-1.11856221181205,-1.37983263907232));
#25824=CARTESIAN_POINT('Ctrl Pts',(99.5271077231788,-1.11276659650673,-1.38451075799837));
#25825=CARTESIAN_POINT('Ctrl Pts',(99.5283704100267,-1.09801839484495,-1.39626281538049));
#25826=CARTESIAN_POINT('Ctrl Pts',(99.5291284701099,-1.08902656769191,-1.40328735364925));
#25827=CARTESIAN_POINT('Ctrl Pts',(99.5322371657803,-1.05161410817432,-1.43193826852985));
#25828=CARTESIAN_POINT('Ctrl Pts',(99.5345403861176,-1.02261016355933,-1.45279327288942));
#25829=CARTESIAN_POINT('Ctrl Pts',(99.5410686892214,-0.937396972408941,
-1.51024744135645));
#25830=CARTESIAN_POINT('Ctrl Pts',(99.5452028114585,-0.879716984612754,
-1.5445580849568));
#25831=CARTESIAN_POINT('Ctrl Pts',(99.5571705698544,-0.706942612411793,
-1.63450576244057));
#25832=CARTESIAN_POINT('Ctrl Pts',(99.5649597770886,-0.587635972053866,
-1.68108800140466));
#25833=CARTESIAN_POINT('Ctrl Pts',(99.5747368687377,-0.441255290506512,
-1.72073570980605));
#25834=CARTESIAN_POINT('Ctrl Pts',(99.5762941741049,-0.418015931223066,
-1.72652836876657));
#25835=CARTESIAN_POINT('Ctrl Pts',(99.57888080784,-0.379600569687917,-1.73528276347286));
#25836=CARTESIAN_POINT('Ctrl Pts',(99.5799013564955,-0.364489968487033,
-1.73851945614003));
#25837=CARTESIAN_POINT('Ctrl Pts',(99.5817647772732,-0.336996623264775,
-1.74403434989305));
#25838=CARTESIAN_POINT('Ctrl Pts',(99.5826054707985,-0.324628107014912,
-1.74637885803619));
#25839=CARTESIAN_POINT('Ctrl Pts',(99.5844360142161,-0.297780001545141,
-1.75117297027572));
#25840=CARTESIAN_POINT('Ctrl Pts',(99.5854273162199,-0.283292957181344,
-1.75357485695897));
#25841=CARTESIAN_POINT('Ctrl Pts',(99.5882374014438,-0.242383623576375,
-1.75983727631489));
#25842=CARTESIAN_POINT('Ctrl Pts',(99.5900690870497,-0.215902653926874,
-1.76328187455139));
#25843=CARTESIAN_POINT('Ctrl Pts',(99.5982463802858,-0.0985510470303378,
-1.77586371933742));
#25844=CARTESIAN_POINT('Ctrl Pts',(99.6047844694313,-0.00714448441541827,
-1.77858055815757));
#25845=CARTESIAN_POINT('Ctrl Pts',(99.6187152633795,0.18410631529159,-1.76952024871536));
#25846=CARTESIAN_POINT('Ctrl Pts',(99.6261058465728,0.283578968985655,-1.7563258846063));
#25847=CARTESIAN_POINT('Ctrl Pts',(99.6359917403932,0.41823895901789,-1.72672005651326));
#25848=CARTESIAN_POINT('Ctrl Pts',(99.638661994828,0.454803647013667,-1.71745162617049));
#25849=CARTESIAN_POINT('Ctrl Pts',(99.6421078547935,0.502559990141931,-1.70371388540186));
#25850=CARTESIAN_POINT('Ctrl Pts',(99.642932833974,0.514038270888048,-1.70028592385774));
#25851=CARTESIAN_POINT('Ctrl Pts',(99.6442685228136,0.532709532106138,-1.6945034299695));
#25852=CARTESIAN_POINT('Ctrl Pts',(99.6447830490297,0.539923475066438,-1.69221865203481));
#25853=CARTESIAN_POINT('Ctrl Pts',(99.6458020449293,0.554257689050783,-1.68757776708112));
#25854=CARTESIAN_POINT('Ctrl Pts',(99.6463065436914,0.561378053054144,-1.6852225348353));
#25855=CARTESIAN_POINT('Ctrl Pts',(99.647590608685,0.579554388520755,-1.67908228699703));
#25856=CARTESIAN_POINT('Ctrl Pts',(99.6483665187982,0.590588539889225,-1.67523306155811));
#25857=CARTESIAN_POINT('Ctrl Pts',(99.65167105263,0.637755546053814,-1.65825504946743));
#25858=CARTESIAN_POINT('Ctrl Pts',(99.6541443323714,0.67349767890683,-1.64406305052046));
#25859=CARTESIAN_POINT('Ctrl Pts',(99.6614132597729,0.778731644759576,-1.59826946346361));
#25860=CARTESIAN_POINT('Ctrl Pts',(99.6660916153545,0.846679010947396,-1.5633376052402));
#25861=CARTESIAN_POINT('Ctrl Pts',(99.6777899807179,1.01024025450393,-1.46544899385541));
#25862=CARTESIAN_POINT('Ctrl Pts',(99.6848042723125,1.1024038474716,-1.39743626646984));
#25863=CARTESIAN_POINT('Ctrl Pts',(99.6937429759855,1.20560634216282,-1.30467513652625));
#25864=CARTESIAN_POINT('Ctrl Pts',(99.695334491446,1.22347957194752,-1.28792915481132));
#25865=CARTESIAN_POINT('Ctrl Pts',(99.6979654092271,1.2521631673138,-1.2599186120261));
#25866=CARTESIAN_POINT('Ctrl Pts',(99.6989954639974,1.26318170084049,-1.24887127888373));
#25867=CARTESIAN_POINT('Ctrl Pts',(99.7008680235581,1.28282208906133,-1.22865370659812));
#25868=CARTESIAN_POINT('Ctrl Pts',(99.7017082223326,1.29149481100285,-1.21953416599933));
#25869=CARTESIAN_POINT('Ctrl Pts',(99.7035282682852,1.30997696920059,-1.19968154373612));
#25870=CARTESIAN_POINT('Ctrl Pts',(99.7045094603304,1.31975292581889,-1.18891869320682));
#25871=CARTESIAN_POINT('Ctrl Pts',(99.7072634834585,1.34666338271397,-1.15855069276903));
#25872=CARTESIAN_POINT('Ctrl Pts',(99.7090484322009,1.3634999659923,-1.13868770583191));
#25873=CARTESIAN_POINT('Ctrl Pts',(99.7168278763477,1.43425942801717,-1.05138886750474));
#25874=CARTESIAN_POINT('Ctrl Pts',(99.7229935416995,1.48365521374533,-0.98044992566828));
#25875=CARTESIAN_POINT('Ctrl Pts',(99.7390288130308,1.59629557601057,-0.79056043226644));
#25876=CARTESIAN_POINT('Ctrl Pts',(99.7490176642994,1.65154522841434,-0.667492573692244));
#25877=CARTESIAN_POINT('Ctrl Pts',(99.7596586726682,1.69766493002482,-0.522781801265699));
#25878=CARTESIAN_POINT('Ctrl Pts',(99.7608674685648,1.70270649283093,-0.506120225278715));
#25879=CARTESIAN_POINT('Ctrl Pts',(99.7626612353024,1.70990012536191,-0.481021154106113));
#25880=CARTESIAN_POINT('Ctrl Pts',(99.7632558419026,1.71223626194066,-0.472638107588769));
#25881=CARTESIAN_POINT('Ctrl Pts',(99.7642810533036,1.71618127765296,-0.458068486587766));
#25882=CARTESIAN_POINT('Ctrl Pts',(99.7647132303375,1.71781846469908,-0.451890077013478));
#25883=CARTESIAN_POINT('Ctrl Pts',(99.7657333970947,1.72162137440022,-0.437219291168476));
#25884=CARTESIAN_POINT('Ctrl Pts',(99.7663197064307,1.72375764248461,-0.428719562719988));
#25885=CARTESIAN_POINT('Ctrl Pts',(99.7680802292582,1.73001878357742,-0.403004273451283));
#25886=CARTESIAN_POINT('Ctrl Pts',(99.7692440941399,1.7339494347153,-0.385741950330786));
#25887=CARTESIAN_POINT('Ctrl Pts',(99.7750666825079,1.75250225611509,-0.298239851186436));
#25888=CARTESIAN_POINT('Ctrl Pts',(99.7795450193971,1.763118914875,-0.227211598628625));
#25889=CARTESIAN_POINT('Ctrl Pts',(99.7862063381242,1.77257983483769,-0.119715507923802));
#25890=CARTESIAN_POINT('Ctrl Pts',(99.7884223183664,1.77464721044379,-0.0836365264494882));
#25891=CARTESIAN_POINT('Ctrl Pts',(99.7906385404719,1.77561363837197,-0.0475422940912529));
#25892=CARTESIAN_POINT('Origin',(88.3562164250559,0.,0.));
#25893=CARTESIAN_POINT('',(100.349869898682,-0.11727379276914,-1.77237437355361));
#25894=CARTESIAN_POINT('Ctrl Pts',(99.7906385404719,1.77561363837197,-0.0475422940912529));
#25895=CARTESIAN_POINT('Ctrl Pts',(99.7964931379277,1.7781666525646,0.0478078968502291));
#25896=CARTESIAN_POINT('Ctrl Pts',(99.8023587123669,1.77303685265072,0.143263940921935));
#25897=CARTESIAN_POINT('Ctrl Pts',(99.8107947900208,1.75531046788573,0.274421537102804));
#25898=CARTESIAN_POINT('Ctrl Pts',(99.8131725253114,1.74923995707394,0.310775302863875));
#25899=CARTESIAN_POINT('Ctrl Pts',(99.8166590559928,1.73884174739516,0.362990650705894));
#25900=CARTESIAN_POINT('Ctrl Pts',(99.8177394055839,1.73541749313107,0.379023653154207));
#25901=CARTESIAN_POINT('Ctrl Pts',(99.8196698378899,1.7289457704255,0.407396722334368));
#25902=CARTESIAN_POINT('Ctrl Pts',(99.8205170332232,1.72598681844863,0.419755946467089));
#25903=CARTESIAN_POINT('Ctrl Pts',(99.8223018592488,1.71950719328883,0.445592975642046));
#25904=CARTESIAN_POINT('Ctrl Pts',(99.8232402929298,1.71596009639686,0.459063193945807));
#25905=CARTESIAN_POINT('Ctrl Pts',(99.8257451941639,1.70612447016286,0.494706490924222));
#25906=CARTESIAN_POINT('Ctrl Pts',(99.8273204131688,1.69956236915572,0.51680062505471));
#25907=CARTESIAN_POINT('Ctrl Pts',(99.8371210260799,1.65644934391702,0.652244844617913));
#25908=CARTESIAN_POINT('Ctrl Pts',(99.8457053012009,1.6090108339211,0.761788915842328));
#25909=CARTESIAN_POINT('Ctrl Pts',(99.8622288396868,1.49878525081889,0.95925809194317));
#25910=CARTESIAN_POINT('Ctrl Pts',(99.8701051645889,1.43823314635055,1.04786563122638));
#25911=CARTESIAN_POINT('Ctrl Pts',(99.8788255728269,1.35900400659355,1.14388552079713));
#25912=CARTESIAN_POINT('Ctrl Pts',(99.880032118174,1.34774881689578,1.15712538543225));
#25913=CARTESIAN_POINT('Ctrl Pts',(99.88182385533,1.33056559766765,1.17674765100802));
#25914=CARTESIAN_POINT('Ctrl Pts',(99.8824186231808,1.32478233477899,1.18325467138048));
#25915=CARTESIAN_POINT('Ctrl Pts',(99.8834451532781,1.31465846148942,1.19447824188463));
#25916=CARTESIAN_POINT('Ctrl Pts',(99.8838784755474,1.3103399516301,1.19921405715651));
#25917=CARTESIAN_POINT('Ctrl Pts',(99.8849028899476,1.30002390826394,1.21040469578874));
#25918=CARTESIAN_POINT('Ctrl Pts',(99.8854922784282,1.29400386830803,1.21683839792716));
#25919=CARTESIAN_POINT('Ctrl Pts',(99.887266350407,1.27563525445852,1.23617871322627));
#25920=CARTESIAN_POINT('Ctrl Pts',(99.8884405157298,1.26313922334615,1.24894454465055));
#25921=CARTESIAN_POINT('Ctrl Pts',(99.8943601328358,1.19854138109877,1.31297562898711));
#25922=CARTESIAN_POINT('Ctrl Pts',(99.8989193420682,1.14349806820828,1.36118365845796));
#25923=CARTESIAN_POINT('Ctrl Pts',(99.9118385786317,0.977832497260549,1.48911351408132));
#25924=CARTESIAN_POINT('Ctrl Pts',(99.9200734028822,0.860822258658605,1.5596788529844));
#25925=CARTESIAN_POINT('Ctrl Pts',(99.9308564995049,0.707663326519199,1.62951195839032));
#25926=CARTESIAN_POINT('Ctrl Pts',(99.9329377705117,0.678071051601471,1.64204629957554));
#25927=CARTESIAN_POINT('Ctrl Pts',(99.936079338257,0.633489645552694,1.65951893390905));
#25928=CARTESIAN_POINT('Ctrl Pts',(99.937119141254,0.618747359725876,1.66507174057476));
#25929=CARTESIAN_POINT('Ctrl Pts',(99.9390041654468,0.592059809403849,1.67472047197822));
#25930=CARTESIAN_POINT('Ctrl Pts',(99.9398469900029,0.580140901425605,1.67888653504072));
#25931=CARTESIAN_POINT('Ctrl Pts',(99.9416669293301,0.554440053742645,1.68756349768375));
#25932=CARTESIAN_POINT('Ctrl Pts',(99.9426453277446,0.540645338890821,1.69203337074829));
#25933=CARTESIAN_POINT('Ctrl Pts',(99.9453754435427,0.502224343950848,1.70396504131501));
#25934=CARTESIAN_POINT('Ctrl Pts',(99.9471388696398,0.477489164643469,1.71106111244297));
#25935=CARTESIAN_POINT('Ctrl Pts',(99.9547220431117,0.371519166192495,1.73898529049829));
#25936=CARTESIAN_POINT('Ctrl Pts',(99.9607023952819,0.289028596435848,1.75458122753618));
#25937=CARTESIAN_POINT('Ctrl Pts',(99.9758780197278,0.081262821903158,1.778811285086));
#25938=CARTESIAN_POINT('Ctrl Pts',(99.985173949752,-0.0444159527475959,
1.78011275838108));
#25939=CARTESIAN_POINT('Ctrl Pts',(99.9958587893048,-0.19451352868987,1.76575080219603));
#25940=CARTESIAN_POINT('Ctrl Pts',(99.9976423189186,-0.219787471432643,
1.7627833211611));
#25941=CARTESIAN_POINT('Ctrl Pts',(100.000114885196,-0.255247737791905,
1.75784524555791));
#25942=CARTESIAN_POINT('Ctrl Pts',(100.000825719795,-0.265492664041288,
1.75632712597737));
#25943=CARTESIAN_POINT('Ctrl Pts',(100.00202503367,-0.282873654983778,1.75359600164842));
#25944=CARTESIAN_POINT('Ctrl Pts',(100.002515985675,-0.290016567911134,
1.75242884010167));
#25945=CARTESIAN_POINT('Ctrl Pts',(100.003538950127,-0.304961934473112,
1.74989286107541));
#25946=CARTESIAN_POINT('Ctrl Pts',(100.004070480329,-0.312762670649016,
1.74851546311266));
#25947=CARTESIAN_POINT('Ctrl Pts',(100.005518719217,-0.334104275838643,
1.74459972001398));
#25948=CARTESIAN_POINT('Ctrl Pts',(100.006429700227,-0.347625568253119,
1.74195589601152));
#25949=CARTESIAN_POINT('Ctrl Pts',(100.012153421272,-0.43308167373984,1.72421193189544));
#25950=CARTESIAN_POINT('Ctrl Pts',(100.016756745132,-0.504060492846061,
1.70481441871399));
#25951=CARTESIAN_POINT('Ctrl Pts',(100.02867172964,-0.686569426825445,1.64253596242109));
#25952=CARTESIAN_POINT('Ctrl Pts',(100.035870955795,-0.795323744137146,
1.59272145887288));
#25953=CARTESIAN_POINT('Ctrl Pts',(100.046476249517,-0.94060713377943,1.50755812215496));
#25954=CARTESIAN_POINT('Ctrl Pts',(100.049612366414,-0.981901512499782,
1.48099359455273));
#25955=CARTESIAN_POINT('Ctrl Pts',(100.054038846053,-1.03744670155824,1.44191651361706));
#25956=CARTESIAN_POINT('Ctrl Pts',(100.055275417571,-1.05267907079813,1.43083388963728));
#25957=CARTESIAN_POINT('Ctrl Pts',(100.057295797944,-1.07708780796221,1.41247406189004));
#25958=CARTESIAN_POINT('Ctrl Pts',(100.058073789185,-1.08637377432647,1.4053444890062));
#25959=CARTESIAN_POINT('Ctrl Pts',(100.059715485944,-1.10572718867635,1.39017889607518));
#25960=CARTESIAN_POINT('Ctrl Pts',(100.060579913049,-1.11577901766145,1.38212414325002));
#25961=CARTESIAN_POINT('Ctrl Pts',(100.062673981084,-1.13979101463918,1.36245013697342));
#25962=CARTESIAN_POINT('Ctrl Pts',(100.063907900593,-1.15366204688499,1.3507249058492));
#25963=CARTESIAN_POINT('Ctrl Pts',(100.068431585451,-1.20349248880167,1.30727551335372));
#25964=CARTESIAN_POINT('Ctrl Pts',(100.071772331565,-1.23834035196693,1.2743138762924));
#25965=CARTESIAN_POINT('Ctrl Pts',(100.080716097545,-1.32655504491058,1.18383517070582));
#25966=CARTESIAN_POINT('Ctrl Pts',(100.08640116284,-1.37751662942011,1.12412620287644));
#25967=CARTESIAN_POINT('Ctrl Pts',(100.100193513115,-1.49029171226726,0.972764769369427));
#25968=CARTESIAN_POINT('Ctrl Pts',(100.108322645641,-1.54783656701778,0.878320211017495));
#25969=CARTESIAN_POINT('Ctrl Pts',(100.117253056011,-1.6037611972641,0.763745715978466));
#25970=CARTESIAN_POINT('Ctrl Pts',(100.118442500313,-1.61105239074613,0.748243105745587));
#25971=CARTESIAN_POINT('Ctrl Pts',(100.12021206701,-1.62167681018176,0.724777766537858));
#25972=CARTESIAN_POINT('Ctrl Pts',(100.120801525421,-1.62517791596065,0.716892765267462));
#25973=CARTESIAN_POINT('Ctrl Pts',(100.121865493586,-1.63143048744985,0.702529823315676));
#25974=CARTESIAN_POINT('Ctrl Pts',(100.122341090928,-1.63420099995054,0.696060832479135));
#25975=CARTESIAN_POINT('Ctrl Pts',(100.123431519087,-1.64049557533343,0.681118590770222));
#25976=CARTESIAN_POINT('Ctrl Pts',(100.124044738171,-1.64399251618068,0.672634286469225));
#25977=CARTESIAN_POINT('Ctrl Pts',(100.125970939406,-1.65483375951348,0.645741497425132));
#25978=CARTESIAN_POINT('Ctrl Pts',(100.12727059158,-1.66193609061336,0.627236290186909));
#25979=CARTESIAN_POINT('Ctrl Pts',(100.130365537081,-1.67828239749075,0.582417273933465));
#25980=CARTESIAN_POINT('Ctrl Pts',(100.13214689171,-1.68721950536279,0.555996578154497));
#25981=CARTESIAN_POINT('Ctrl Pts',(100.139388530913,-1.72137497511728,0.446600285214749));
#25982=CARTESIAN_POINT('Ctrl Pts',(100.144677507945,-1.7411241685882,0.362038905240627));
#25983=CARTESIAN_POINT('Ctrl Pts',(100.156192531159,-1.77028828940717,0.176880812480538));
#25984=CARTESIAN_POINT('Ctrl Pts',(100.1624167039,-1.77746729641969,0.0762515473305784));
#25985=CARTESIAN_POINT('Ctrl Pts',(100.170503652907,-1.7757399584398,-0.049288293428972));
#25986=CARTESIAN_POINT('Ctrl Pts',(100.172118675183,-1.77487652381352,-0.0741280254872288));
#25987=CARTESIAN_POINT('Ctrl Pts',(100.174783874909,-1.77261439996511,-0.11467621371666));
#25988=CARTESIAN_POINT('Ctrl Pts',(100.175824420483,-1.77152716548375,-0.130399081014327));
#25989=CARTESIAN_POINT('Ctrl Pts',(100.177713247363,-1.76918879768221,-0.158731110894724));
#25990=CARTESIAN_POINT('Ctrl Pts',(100.1785591612,-1.76801167852979,-0.171345434039105));
#25991=CARTESIAN_POINT('Ctrl Pts',(100.180388596644,-1.76518858407098,-0.198459725023159));
#25992=CARTESIAN_POINT('Ctrl Pts',(100.181373437265,-1.76349866436725,-0.212954076099071));
#25993=CARTESIAN_POINT('Ctrl Pts',(100.18412998137,-1.75829911352762,-0.253229608198164));
#25994=CARTESIAN_POINT('Ctrl Pts',(100.18591364563,-1.75440143670731,-0.278956057226832));
#25995=CARTESIAN_POINT('Ctrl Pts',(100.193654462878,-1.73522562382617,-0.389126828354918));
#25996=CARTESIAN_POINT('Ctrl Pts',(100.199778930604,-1.71440618092535,-0.472477938770434));
#25997=CARTESIAN_POINT('Ctrl Pts',(100.215758291561,-1.64573007071061,-0.681690225334595));
#25998=CARTESIAN_POINT('Ctrl Pts',(100.225732072662,-1.58945147911387,-0.804223648557327));
#25999=CARTESIAN_POINT('Ctrl Pts',(100.236360272327,-1.51089579874509,-0.934109162755003));
#26000=CARTESIAN_POINT('Ctrl Pts',(100.237566452318,-1.50168445839896,-0.948846608274311));
#26001=CARTESIAN_POINT('Ctrl Pts',(100.239360746398,-1.48751214229155,-0.970797734955737));
#26002=CARTESIAN_POINT('Ctrl Pts',(100.239958336748,-1.48271201375453,-0.978113341094658));
#26003=CARTESIAN_POINT('Ctrl Pts',(100.241044264017,-1.47383879528095,-0.991421078291027));
#26004=CARTESIAN_POINT('Ctrl Pts',(100.241533627991,-1.46978298334533,-0.997423948534114));
#26005=CARTESIAN_POINT('Ctrl Pts',(100.24265665706,-1.46034494559226,-1.01121028597273));
#26006=CARTESIAN_POINT('Ctrl Pts',(100.243288632095,-1.45493709641348,-1.01897578867778));
#26007=CARTESIAN_POINT('Ctrl Pts',(100.245298897122,-1.43743486561957,-1.04368501502761));
#26008=CARTESIAN_POINT('Ctrl Pts',(100.246662715023,-1.42510411452673,-1.06046016221564));
#26009=CARTESIAN_POINT('Ctrl Pts',(100.249940084928,-1.39444202574328,-1.10067277560797));
#26010=CARTESIAN_POINT('Ctrl Pts',(100.251837960713,-1.37581088016087,-1.12387443024082));
#26011=CARTESIAN_POINT('Ctrl Pts',(100.260015852776,-1.29218072667421,-1.2228219534349));
#26012=CARTESIAN_POINT('Ctrl Pts',(100.266086711509,-1.22144413596312,-1.2934840281648));
#26013=CARTESIAN_POINT('Ctrl Pts',(100.277662150094,-1.07847096798431,-1.41406198557683));
#26014=CARTESIAN_POINT('Ctrl Pts',(100.283125091899,-1.00775549094225,-1.46529764574405));
#26015=CARTESIAN_POINT('Ctrl Pts',(100.290221680105,-0.914734817061573,
-1.52276537288529));
#26016=CARTESIAN_POINT('Ctrl Pts',(100.291670065379,-0.895685677918712,
-1.53404734704009));
#26017=CARTESIAN_POINT('Ctrl Pts',(100.294045044164,-0.864386076516734,
-1.55180300017576));
#26018=CARTESIAN_POINT('Ctrl Pts',(100.294963867128,-0.852261632047777,
-1.5584947651689));
#26019=CARTESIAN_POINT('Ctrl Pts',(100.296752076926,-0.828644702208023,
-1.57117150139329));
#26020=CARTESIAN_POINT('Ctrl Pts',(100.297620782814,-0.817162507140867,
-1.57717384932715));
#26021=CARTESIAN_POINT('Ctrl Pts',(100.299673488765,-0.790016696886263,
-1.59098838352615));
#26022=CARTESIAN_POINT('Ctrl Pts',(100.300861028043,-0.774301481547401,
-1.59869559191857));
#26023=CARTESIAN_POINT('Ctrl Pts',(100.304918676448,-0.720588396485923,
-1.6240603277503));
#26024=CARTESIAN_POINT('Ctrl Pts',(100.30782579467,-0.682083190217163,-1.64060403581061));
#26025=CARTESIAN_POINT('Ctrl Pts',(100.31520079313,-0.58440537653619,-1.67853801187126));
#26026=CARTESIAN_POINT('Ctrl Pts',(100.319716751716,-0.524616485653908,
-1.6981742315184));
#26027=CARTESIAN_POINT('Ctrl Pts',(100.332814292871,-0.350563757656464,
-1.74526754135083));
#26028=CARTESIAN_POINT('Ctrl Pts',(100.341510471993,-0.234449217791222,
-1.76462115464189));
#26029=CARTESIAN_POINT('Ctrl Pts',(100.349869898682,-0.11727379276914,-1.77237437355361));
#26030=CARTESIAN_POINT('',(100.349869898682,-1.70764710160359,-0.4888818250711));
#26031=CARTESIAN_POINT('Origin',(100.349869898682,0.,0.));
#26032=CARTESIAN_POINT('',(100.129086829157,0.00137221428264897,1.77624946995853));
#26033=CARTESIAN_POINT('Ctrl Pts',(100.128149994198,0.00130396094780403,
1.77624952137526));
#26034=CARTESIAN_POINT('Ctrl Pts',(100.135254863005,-0.0957291980175613,
1.77632075430082));
#26035=CARTESIAN_POINT('Ctrl Pts',(100.142452083519,-0.192611897045183,
1.76844057705337));
#26036=CARTESIAN_POINT('Ctrl Pts',(100.153400526873,-0.341559757154774,
1.74393434377953));
#26037=CARTESIAN_POINT('Ctrl Pts',(100.157258709097,-0.394330021920698,
1.73276509497843));
#26038=CARTESIAN_POINT('Ctrl Pts',(100.163670309496,-0.482710034608528,
1.70981096361842));
#26039=CARTESIAN_POINT('Ctrl Pts',(100.166260022626,-0.518601382447507,
1.69926910775185));
#26040=CARTESIAN_POINT('Ctrl Pts',(100.16991347725,-0.569481615602692,1.68256222428895));
#26041=CARTESIAN_POINT('Ctrl Pts',(100.171008143872,-0.584758490520812,
1.67731406971457));
#26042=CARTESIAN_POINT('Ctrl Pts',(100.17290921631,-0.611336589015278,1.66777626711555));
#26043=CARTESIAN_POINT('Ctrl Pts',(100.173718736893,-0.622669344120547,
1.66357837301651));
#26044=CARTESIAN_POINT('Ctrl Pts',(100.175391216247,-0.646108810887612,
1.65462281025941));
#26045=CARTESIAN_POINT('Ctrl Pts',(100.176253489696,-0.658207907909286,
1.64984714612651));
#26046=CARTESIAN_POINT('Ctrl Pts',(100.178490484007,-0.689623498788055,
1.63704641687366));
#26047=CARTESIAN_POINT('Ctrl Pts',(100.179857819311,-0.708852990212084,
1.6288121567253));
#26048=CARTESIAN_POINT('Ctrl Pts',(100.186204135166,-0.798129580645457,
1.58870241649473));
#26049=CARTESIAN_POINT('Ctrl Pts',(100.191033393552,-0.866206930111896,
1.55263449281232));
#26050=CARTESIAN_POINT('Ctrl Pts',(100.202812077758,-1.02848006103079,1.45265444116518));
#26051=CARTESIAN_POINT('Ctrl Pts',(100.209639196324,-1.11927360515802,1.38390744305321));
#26052=CARTESIAN_POINT('Ctrl Pts',(100.218737239276,-1.22586488352479,1.28580545218075));
#26053=CARTESIAN_POINT('Ctrl Pts',(100.220722514642,-1.24829200097628,1.26404399448709));
#26054=CARTESIAN_POINT('Ctrl Pts',(100.223704015737,-1.28051401528967,1.23108426857808));
#26055=CARTESIAN_POINT('Ctrl Pts',(100.224672574085,-1.2907618765233,1.22033534914517));
#26056=CARTESIAN_POINT('Ctrl Pts',(100.226417402782,-1.30880378400833,1.20092979266328));
#26057=CARTESIAN_POINT('Ctrl Pts',(100.227190040689,-1.31664984729168,1.19232247019853));
#26058=CARTESIAN_POINT('Ctrl Pts',(100.228453023708,-1.32923194661045,1.17824396755008));
#26059=CARTESIAN_POINT('Ctrl Pts',(100.22893945945,-1.33402037658051,1.17281969967129));
#26060=CARTESIAN_POINT('Ctrl Pts',(100.229911944483,-1.34347635260876,1.16197526391989));
#26061=CARTESIAN_POINT('Ctrl Pts',(100.2303978796,-1.34814446962376,1.15655596851853));
#26062=CARTESIAN_POINT('Ctrl Pts',(100.231586371648,-1.35942674043813,1.14329707703154));
#26063=CARTESIAN_POINT('Ctrl Pts',(100.232291379014,-1.3660058696929,1.13542820998825));
#26064=CARTESIAN_POINT('Ctrl Pts',(100.23469829316,-1.38809593824661,1.10853783602053));
#26065=CARTESIAN_POINT('Ctrl Pts',(100.236420556478,-1.40327988636873,1.08925289997557));
#26066=CARTESIAN_POINT('Ctrl Pts',(100.240873730137,-1.44107521640734,1.03914730809804));
#26067=CARTESIAN_POINT('Ctrl Pts',(100.243630531566,-1.46309966175944,1.00790074423885));
#26068=CARTESIAN_POINT('Ctrl Pts',(100.257223945286,-1.56571370811657,0.851861914884223));
#26069=CARTESIAN_POINT('Ctrl Pts',(100.268300822581,-1.63145237939817,0.717983898341546));
#26070=CARTESIAN_POINT('Ctrl Pts',(100.283007746724,-1.69847099997986,0.523043288335931));
#26071=CARTESIAN_POINT('Ctrl Pts',(100.287043275869,-1.71453080141143,0.467721480528988));
#26072=CARTESIAN_POINT('Ctrl Pts',(100.292459079198,-1.73280383288821,0.391033029518842));
#26073=CARTESIAN_POINT('Ctrl Pts',(100.293908267301,-1.73735965123781,0.370266741216327));
#26074=CARTESIAN_POINT('Ctrl Pts',(100.296231649236,-1.74411536231491,0.336595930652565));
#26075=CARTESIAN_POINT('Ctrl Pts',(100.29711255254,-1.74654723182124,0.323740635635537));
#26076=CARTESIAN_POINT('Ctrl Pts',(100.29895096592,-1.75134785091464,0.296733246809969));
#26077=CARTESIAN_POINT('Ctrl Pts',(100.29990758161,-1.75368760646362,0.282576913609874));
#26078=CARTESIAN_POINT('Ctrl Pts',(100.302203418469,-1.7589165702476,0.248368533556482));
#26079=CARTESIAN_POINT('Ctrl Pts',(100.303537768131,-1.76163480209468,0.228292142238424));
#26080=CARTESIAN_POINT('Ctrl Pts',(100.308235613119,-1.77004853425795,0.156996165263256));
#26081=CARTESIAN_POINT('Ctrl Pts',(100.311548657578,-1.77385835962502,0.105578141115755));
#26082=CARTESIAN_POINT('Ctrl Pts',(100.319609588662,-1.77771670573629,-0.0211273285827478));
#26083=CARTESIAN_POINT('Ctrl Pts',(100.324307062743,-1.77522748861565,-0.0963891624062148));
#26084=CARTESIAN_POINT('Ctrl Pts',(100.334017882365,-1.76031064369582,-0.250373579713448));
#26085=CARTESIAN_POINT('Ctrl Pts',(100.339023932768,-1.7473475234668,-0.32886927391282));
#26086=CARTESIAN_POINT('Ctrl Pts',(100.345236306438,-1.72559434857467,-0.421465625819561));
#26087=CARTESIAN_POINT('Ctrl Pts',(100.346265671596,-1.72181296112772,-0.436656873573249));
#26088=CARTESIAN_POINT('Ctrl Pts',(100.347762245216,-1.71607028779066,-0.458491843083625));
#26089=CARTESIAN_POINT('Ctrl Pts',(100.348222803322,-1.71427006020475,-0.465177557974144));
#26090=CARTESIAN_POINT('Ctrl Pts',(100.349078977483,-1.71086361427569,-0.477540114841893));
#26091=CARTESIAN_POINT('Ctrl Pts',(100.349473448819,-1.70927082021505,-0.483210232799742));
#26092=CARTESIAN_POINT('Ctrl Pts',(100.349869898682,-1.70764710160359,-0.4888818250711));
#26093=CARTESIAN_POINT('Ctrl Pts',(99.938371422543,1.77561385491717,-0.0475342058543041));
#26094=CARTESIAN_POINT('Ctrl Pts',(99.9429651167472,1.7774525533391,0.0211493523185398));
#26095=CARTESIAN_POINT('Ctrl Pts',(99.9475588109513,1.77529901241746,0.089836337665965));
#26096=CARTESIAN_POINT('Ctrl Pts',(99.9521525051555,1.76920256918782,0.158070654073485));
#26097=CARTESIAN_POINT('Ctrl Pts',(99.9567561361381,1.76309293853142,0.226452570485825));
#26098=CARTESIAN_POINT('Ctrl Pts',(99.9613597671207,1.7530234469905,0.294379482442791));
#26099=CARTESIAN_POINT('Ctrl Pts',(99.9659633981033,1.73909474169064,0.361404955588548));
#26100=CARTESIAN_POINT('Ctrl Pts',(99.9705844437525,1.72511334672927,0.428683973440486));
#26101=CARTESIAN_POINT('Ctrl Pts',(99.9752054894016,1.70724363047171,0.495054354679337));
#26102=CARTESIAN_POINT('Ctrl Pts',(99.9798265350508,1.68563674621482,0.560082870931005));
#26103=CARTESIAN_POINT('Ctrl Pts',(99.9840236069088,1.66601226016998,0.619145121393658));
#26104=CARTESIAN_POINT('Ctrl Pts',(99.9882206787669,1.64330561823309,0.677100483889278));
#26105=CARTESIAN_POINT('Ctrl Pts',(99.9924177506249,1.61766340334978,0.733641040266147));
#26106=CARTESIAN_POINT('Ctrl Pts',(99.996719443715,1.59138199995517,0.791590994162829));
#26107=CARTESIAN_POINT('Ctrl Pts',(100.001021136805,1.56193031631559,0.848242522556317));
#26108=CARTESIAN_POINT('Ctrl Pts',(100.005322829895,1.52945925765464,0.903226683438055));
#26109=CARTESIAN_POINT('Ctrl Pts',(100.009749731426,1.49604307098206,0.959811256280128));
#26110=CARTESIAN_POINT('Ctrl Pts',(100.014176632958,1.45942912853903,1.01462935526712));
#26111=CARTESIAN_POINT('Ctrl Pts',(100.018603534489,1.4198350438754,1.0673015087984));
#26112=CARTESIAN_POINT('Ctrl Pts',(100.022893633379,1.38146451824141,1.11834595734265));
#26113=CARTESIAN_POINT('Ctrl Pts',(100.02718373227,1.34029569218185,1.1673747307569));
#26114=CARTESIAN_POINT('Ctrl Pts',(100.03147383116,1.29657165064649,1.21407002155552));
#26115=CARTESIAN_POINT('Ctrl Pts',(100.035761382289,1.25287357550642,1.26073758142316));
#26116=CARTESIAN_POINT('Ctrl Pts',(100.040048933419,1.20662363749741,1.30507404058467));
#26117=CARTESIAN_POINT('Ctrl Pts',(100.044336484548,1.15810445639107,1.34679550436848));
#26118=CARTESIAN_POINT('Ctrl Pts',(100.048623025896,1.10959670226696,1.38850714213267));
#26119=CARTESIAN_POINT('Ctrl Pts',(100.052909567244,1.05882114733742,1.4276046794328));
#26120=CARTESIAN_POINT('Ctrl Pts',(100.057196108593,1.00609497862374,1.4638432144489));
#26121=CARTESIAN_POINT('Ctrl Pts',(100.061483176441,0.953362333746309,1.50008620051262));
#26122=CARTESIAN_POINT('Ctrl Pts',(100.065770244289,0.898679015852326,1.5334692051429));
#26123=CARTESIAN_POINT('Ctrl Pts',(100.070057312138,0.842391150091806,1.56379065502611));
#26124=CARTESIAN_POINT('Ctrl Pts',(100.074349204795,0.786039936085563,1.59414622968262));
#26125=CARTESIAN_POINT('Ctrl Pts',(100.078641097453,0.728081015997666,1.62143313850311));
#26126=CARTESIAN_POINT('Ctrl Pts',(100.082932990111,0.668883993757652,1.64549635836571));
#26127=CARTESIAN_POINT('Ctrl Pts',(100.087227806043,0.609646651508125,1.66957596806038));
#26128=CARTESIAN_POINT('Ctrl Pts',(100.091522621976,0.549170004807765,1.69042735741353));
#26129=CARTESIAN_POINT('Ctrl Pts',(100.095817437908,0.487839665905936,1.70794511705405));
#26130=CARTESIAN_POINT('Ctrl Pts',(100.100119519895,0.42640556712641,1.72549251358605));
#26131=CARTESIAN_POINT('Ctrl Pts',(100.104421601882,0.364115384978533,1.7396949214122));
#26132=CARTESIAN_POINT('Ctrl Pts',(100.108723683869,0.301364584863964,1.75049805755098));
#26133=CARTESIAN_POINT('Ctrl Pts',(100.109671944794,0.287533111647908,1.75287927480846));
#26134=CARTESIAN_POINT('Ctrl Pts',(100.110620205719,0.273679273198215,1.75509554040592));
#26135=CARTESIAN_POINT('Ctrl Pts',(100.111568466644,0.259807318327067,1.75714661307578));
#26136=CARTESIAN_POINT('Ctrl Pts',(100.117407920815,0.174382892857341,1.76977725569591));
#26137=CARTESIAN_POINT('Ctrl Pts',(100.123247374986,0.0880030702956733,
1.77618254461952));
#26138=CARTESIAN_POINT('Ctrl Pts',(100.129086829157,0.00137221428264898,
1.77624946995853));
#26139=CARTESIAN_POINT('Origin',(70.8,0.,0.));
#26140=CARTESIAN_POINT('',(69.8,0.,1.22464679914735E-16));
#26141=CARTESIAN_POINT('Origin',(70.8,0.,0.));
#26142=CARTESIAN_POINT('',(69.8,0.,1.22464679914735E-16));
#26143=CARTESIAN_POINT('Origin',(70.8,0.,0.));
#26144=CARTESIAN_POINT('Origin',(66.9212607628943,0.,0.));
#26145=CARTESIAN_POINT('',(100.349820515151,0.479516069206331,2.15120439274675));
#26146=CARTESIAN_POINT('Ctrl Pts',(99.6260484068026,-0.00167252030352779,
2.20399936539824));
#26147=CARTESIAN_POINT('Ctrl Pts',(99.6319075205934,-0.109497489706828,
2.20391754166753));
#26148=CARTESIAN_POINT('Ctrl Pts',(99.6377666343843,-0.217027700916224,
2.19592210702929));
#26149=CARTESIAN_POINT('Ctrl Pts',(99.6436257481752,-0.323376599163019,
2.18014760397404));
#26150=CARTESIAN_POINT('Ctrl Pts',(99.6476982151888,-0.397296033995319,
2.16918329339042));
#26151=CARTESIAN_POINT('Ctrl Pts',(99.6517706822024,-0.470800001612205,
2.15443410450263));
#26152=CARTESIAN_POINT('Ctrl Pts',(99.655843149216,-0.543470878609583,2.1359436799933));
#26153=CARTESIAN_POINT('Ctrl Pts',(99.6599096309551,-0.616034951759509,
2.11748043072336));
#26154=CARTESIAN_POINT('Ctrl Pts',(99.6639761126941,-0.687767906160161,
2.09528697922465));
#26155=CARTESIAN_POINT('Ctrl Pts',(99.6680425944332,-0.758259772046648,
2.06945841178212));
#26156=CARTESIAN_POINT('Ctrl Pts',(99.6721043188555,-0.82866917054216,2.0436600607985));
#26157=CARTESIAN_POINT('Ctrl Pts',(99.6761660432778,-0.897839918948113,
2.01423520635791));
#26158=CARTESIAN_POINT('Ctrl Pts',(99.6802277677001,-0.965376331664208,
1.98132898284524));
#26159=CARTESIAN_POINT('Ctrl Pts',(99.6842869148638,-1.03286989095618,1.94844363909648));
#26160=CARTESIAN_POINT('Ctrl Pts',(99.6883460620275,-1.09873074412541,1.91208151843965));
#26161=CARTESIAN_POINT('Ctrl Pts',(99.6924052091912,-1.16258360835439,1.87243567408488));
#26162=CARTESIAN_POINT('Ctrl Pts',(99.6964630934742,-1.22641660669966,1.83280216433315));
#26163=CARTESIAN_POINT('Ctrl Pts',(99.7005209777573,-1.28824245095615,1.78988721103953));
#26164=CARTESIAN_POINT('Ctrl Pts',(99.7045788620403,-1.34771229727502,1.74392877256317));
#26165=CARTESIAN_POINT('Ctrl Pts',(99.7086367961383,-1.40718287365091,1.69796976989702));
#26166=CARTESIAN_POINT('Ctrl Pts',(99.7126947302363,-1.46429701784226,1.64896750133811));
#26167=CARTESIAN_POINT('Ctrl Pts',(99.7167526643343,-1.51873790819427,1.59720104126365));
#26168=CARTESIAN_POINT('Ctrl Pts',(99.7208147569618,-1.57323458901551,1.54538153144885));
#26169=CARTESIAN_POINT('Ctrl Pts',(99.7248768495893,-1.62505219845158,1.49079250321318));
#26170=CARTESIAN_POINT('Ctrl Pts',(99.7289389422167,-1.67391040222215,1.43375031485));
#26171=CARTESIAN_POINT('Ctrl Pts',(99.7330031604474,-1.72279417240918,1.3766782775724));
#26172=CARTESIAN_POINT('Ctrl Pts',(99.737067378678,-1.76871516112033,1.31715090239909));
#26173=CARTESIAN_POINT('Ctrl Pts',(99.7411315969086,-1.81143468416356,1.25551598357379));
#26174=CARTESIAN_POINT('Ctrl Pts',(99.7452030889128,-1.85423066278052,1.19377075609463));
#26175=CARTESIAN_POINT('Ctrl Pts',(99.7492745809169,-1.89381347915068,1.12991085748517));
#26176=CARTESIAN_POINT('Ctrl Pts',(99.7533460729211,-1.92998920718614,1.06431088510126));
#26177=CARTESIAN_POINT('Ctrl Pts',(99.7564895366788,-1.95791928536689,1.01366332507036));
#26178=CARTESIAN_POINT('Ctrl Pts',(99.7596330004366,-1.9838193552616,0.961979094348991));
#26179=CARTESIAN_POINT('Ctrl Pts',(99.7627764641943,-2.00762000554835,0.909438240521063));
#26180=CARTESIAN_POINT('Ctrl Pts',(99.7668503345384,-2.03846520398165,0.841346274854084));
#26181=CARTESIAN_POINT('Ctrl Pts',(99.7709242048826,-2.06590167641681,0.77155217677183));
#26182=CARTESIAN_POINT('Ctrl Pts',(99.7749980752268,-2.08973983899598,0.700430871187907));
#26183=CARTESIAN_POINT('Ctrl Pts',(99.7790659583805,-2.11354296766243,0.629414089499418));
#26184=CARTESIAN_POINT('Ctrl Pts',(99.7831338415343,-2.13375813556486,0.557074421736932));
#26185=CARTESIAN_POINT('Ctrl Pts',(99.7872017246881,-2.15024315109428,0.483808217346638));
#26186=CARTESIAN_POINT('Ctrl Pts',(99.791264841114,-2.16670884955418,0.410627865976101));
#26187=CARTESIAN_POINT('Ctrl Pts',(99.79532795754,-2.17945297566547,0.336523598353343));
#26188=CARTESIAN_POINT('Ctrl Pts',(99.799391073966,-2.18838314651579,0.261906861394773));
#26189=CARTESIAN_POINT('Ctrl Pts',(99.8034516067101,-2.19730763878879,0.187337572230529));
#26190=CARTESIAN_POINT('Ctrl Pts',(99.8075121394541,-2.2024229319316,0.112256933073733));
#26191=CARTESIAN_POINT('Ctrl Pts',(99.8115726721982,-2.2036879743073,0.0370851977666151));
#26192=CARTESIAN_POINT('Ctrl Pts',(99.8156319337375,-2.20495262064433,-0.0380630040093736));
#26193=CARTESIAN_POINT('Ctrl Pts',(99.8196911952767,-2.20236940143706,-0.113301768433216));
#26194=CARTESIAN_POINT('Ctrl Pts',(99.8237504568159,-2.19594933265433,-0.188208736287638));
#26195=CARTESIAN_POINT('Ctrl Pts',(99.8278097579377,-2.1895292012684,-0.263116434572969));
#26196=CARTESIAN_POINT('Ctrl Pts',(99.8318690590596,-2.17927218856319,-0.337691854502154));
#26197=CARTESIAN_POINT('Ctrl Pts',(99.8359283601814,-2.16524121855838,-0.411517272366319));
#26198=CARTESIAN_POINT('Ctrl Pts',(99.8399917946099,-2.1511959617833,-0.485417861568273));
#26199=CARTESIAN_POINT('Ctrl Pts',(99.8440552290384,-2.13336916319436,-0.558566453773009));
#26200=CARTESIAN_POINT('Ctrl Pts',(99.8481186634669,-2.11187485349889,-0.630555789093284));
#26201=CARTESIAN_POINT('Ctrl Pts',(99.8521842116242,-2.09036936283288,-0.702582572028724));
#26202=CARTESIAN_POINT('Ctrl Pts',(99.8562497597815,-2.0651927217192,-0.773448447030229));
#26203=CARTESIAN_POINT('Ctrl Pts',(99.8603153079388,-2.03650795310874,-0.842764117013095));
#26204=CARTESIAN_POINT('Ctrl Pts',(99.8643880953861,-2.00777210716519,-0.912203213460093));
#26205=CARTESIAN_POINT('Ctrl Pts',(99.8684608828333,-1.97551586144112,-0.980086159530162));
#26206=CARTESIAN_POINT('Ctrl Pts',(99.8725336702806,-1.9399490218486,-1.04604674495391));
#26207=CARTESIAN_POINT('Ctrl Pts',(99.8756648402583,-1.91260513961213,-1.09675742098638));
#26208=CARTESIAN_POINT('Ctrl Pts',(99.8787960102359,-1.88330547707187,-1.14633233670067));
#26209=CARTESIAN_POINT('Ctrl Pts',(99.8819271802136,-1.852162309428,-1.19461741973501));
#26210=CARTESIAN_POINT('Ctrl Pts',(99.8860008808318,-1.81164456615917,-1.25743706032109));
#26211=CARTESIAN_POINT('Ctrl Pts',(99.8900745814501,-1.76784935617139,-1.31831374420271));
#26212=CARTESIAN_POINT('Ctrl Pts',(99.8941482820683,-1.72098914358945,-1.3768850233942));
#26213=CARTESIAN_POINT('Ctrl Pts',(99.8982160097284,-1.67419763858216,-1.43537042396254));
#26214=CARTESIAN_POINT('Ctrl Pts',(99.9022837373885,-1.62435034917707,-1.49155676147313));
#26215=CARTESIAN_POINT('Ctrl Pts',(99.9063514650486,-1.57170341901845,-1.54510982219573));
#26216=CARTESIAN_POINT('Ctrl Pts',(99.9104144477303,-1.51911790116863,-1.59860041361399));
#26217=CARTESIAN_POINT('Ctrl Pts',(99.914477430412,-1.46373956386138,-1.64946349240418));
#26218=CARTESIAN_POINT('Ctrl Pts',(99.9185404130937,-1.40586422196226,-1.69739853582075));
#26219=CARTESIAN_POINT('Ctrl Pts',(99.9226008254423,-1.34802549328917,-1.74530325446479));
#26220=CARTESIAN_POINT('Ctrl Pts',(99.926661237791,-1.287693261377,-1.79028330987578));
#26221=CARTESIAN_POINT('Ctrl Pts',(99.9307216501396,-1.22519854720158,-1.83207655951795));
#26222=CARTESIAN_POINT('Ctrl Pts',(99.9347808046823,-1.16272319219846,-1.87385686274167));
#26223=CARTESIAN_POINT('Ctrl Pts',(99.938839959225,-1.0980870814465,-1.912452055093));
#26224=CARTESIAN_POINT('Ctrl Pts',(99.9428991137678,-1.03165120709997,-1.94764262299046));
#26225=CARTESIAN_POINT('Ctrl Pts',(99.9469583213553,-0.965214464572138,
-1.98283365075684));
#26226=CARTESIAN_POINT('Ctrl Pts',(99.9510175289429,-0.89697833435288,-2.01461974390755));
#26227=CARTESIAN_POINT('Ctrl Pts',(99.9550767365305,-0.82732802653297,-2.04282753469623));
#26228=CARTESIAN_POINT('Ctrl Pts',(99.9591400986934,-0.757606432029038,
-2.07106419599434));
#26229=CARTESIAN_POINT('Ctrl Pts',(99.9632034608563,-0.686468212907689,
-2.09571506184319));
#26230=CARTESIAN_POINT('Ctrl Pts',(99.9672668230191,-0.614317465756464,
-2.11665539265761));
#26231=CARTESIAN_POINT('Ctrl Pts',(99.9713323105909,-0.542128978961985,
-2.13760667665888));
#26232=CARTESIAN_POINT('Ctrl Pts',(99.9753977981627,-0.468927374446688,
-2.15484345107275));
#26233=CARTESIAN_POINT('Ctrl Pts',(99.9794632857344,-0.395128183154033,
-2.16829188968584));
#26234=CARTESIAN_POINT('Ctrl Pts',(99.983536032225,-0.32119722357254,-2.1817643404556));
#26235=CARTESIAN_POINT('Ctrl Pts',(99.9876087787156,-0.246667019992794,
-2.19143488320763));
#26236=CARTESIAN_POINT('Ctrl Pts',(99.9916815252062,-0.171959035827759,
-2.19728152269963));
#26237=CARTESIAN_POINT('Ctrl Pts',(99.9948136488818,-0.114505264399459,
-2.20177784920008));
#26238=CARTESIAN_POINT('Ctrl Pts',(99.9979457725574,-0.0569464831372791,
-2.20401367458827));
#26239=CARTESIAN_POINT('Ctrl Pts',(100.001077896233,0.000526810878827148,
-2.20399993703954));
#26240=CARTESIAN_POINT('Ctrl Pts',(100.0051464063,0.0751824437715719,-2.20398209248387));
#26241=CARTESIAN_POINT('Ctrl Pts',(100.009214916367,0.14998309808274,-2.20016671252712));
#26242=CARTESIAN_POINT('Ctrl Pts',(100.013283426434,0.224509972218602,-2.19253535259398));
#26243=CARTESIAN_POINT('Ctrl Pts',(100.017345940743,0.298927016180346,-2.18491523898775));
#26244=CARTESIAN_POINT('Ctrl Pts',(100.021408455051,0.373070608838928,-2.17349035812419));
#26245=CARTESIAN_POINT('Ctrl Pts',(100.025470969359,0.446521919783342,-2.1582942744568));
#26246=CARTESIAN_POINT('Ctrl Pts',(100.029528729261,0.519887269822233,-2.14311597493915));
#26247=CARTESIAN_POINT('Ctrl Pts',(100.033586489162,0.592561481353539,-2.12417533700807));
#26248=CARTESIAN_POINT('Ctrl Pts',(100.037644249064,0.664132470250156,-2.1015575323934));
#26249=CARTESIAN_POINT('Ctrl Pts',(100.04169943528,0.735658064353487,-2.0789540734037));
#26250=CARTESIAN_POINT('Ctrl Pts',(100.045754621497,0.806081369022975,-2.052678219385));
#26251=CARTESIAN_POINT('Ctrl Pts',(100.049809807713,0.875003427246544,-2.0228655423203));
#26252=CARTESIAN_POINT('Ctrl Pts',(100.053863740074,0.943904174901207,-1.99306208327847));
#26253=CARTESIAN_POINT('Ctrl Pts',(100.057917672435,1.01130415862764,-1.95972416217078));
#26254=CARTESIAN_POINT('Ctrl Pts',(100.061971604796,1.07682397552376,-1.92303565378731));
#26255=CARTESIAN_POINT('Ctrl Pts',(100.066025601453,1.14234483158063,-1.8863465635149));
#26256=CARTESIAN_POINT('Ctrl Pts',(100.07007959811,1.20598504484707,-1.84630701587621));
#26257=CARTESIAN_POINT('Ctrl Pts',(100.074133594767,1.26739085804168,-1.80314625389966));
#26258=CARTESIAN_POINT('Ctrl Pts',(100.078191799491,1.32886041074648,-1.75994069085812));
#26259=CARTESIAN_POINT('Ctrl Pts',(100.082250004215,1.38809053945869,-1.71360771970359));
#26260=CARTESIAN_POINT('Ctrl Pts',(100.086308208939,1.44475811611921,-1.66441881325214));
#26261=CARTESIAN_POINT('Ctrl Pts',(100.090368560473,1.50145567020147,-1.61520388563161));
#26262=CARTESIAN_POINT('Ctrl Pts',(100.094428912007,1.55558762779912,-1.56313034662586));
#26263=CARTESIAN_POINT('Ctrl Pts',(100.09848926354,1.60686747152173,-1.50850685413271));
#26264=CARTESIAN_POINT('Ctrl Pts',(100.102556967611,1.65824017343895,-1.45378444872314));
#26265=CARTESIAN_POINT('Ctrl Pts',(100.106624671681,1.70675013601905,-1.39650323279177));
#26266=CARTESIAN_POINT('Ctrl Pts',(100.110692375751,1.75215120358949,-1.33700492136713));
#26267=CARTESIAN_POINT('Ctrl Pts',(100.113871121251,1.78763029370135,-1.2905094078142));
#26268=CARTESIAN_POINT('Ctrl Pts',(100.117049866752,1.82121165407053,-1.24266065374487));
#26269=CARTESIAN_POINT('Ctrl Pts',(100.120228612252,1.85279711796351,-1.19363262340894));
#26270=CARTESIAN_POINT('Ctrl Pts',(100.124309031285,1.89334202098052,-1.13069744722091));
#26271=CARTESIAN_POINT('Ctrl Pts',(100.128389450318,1.93075359612356,-1.0655746909329));
#26272=CARTESIAN_POINT('Ctrl Pts',(100.13246986935,1.96478922686938,-0.998608679102096));
#26273=CARTESIAN_POINT('Ctrl Pts',(100.136544285542,1.9987747866604,-0.931741183211151));
#26274=CARTESIAN_POINT('Ctrl Pts',(100.140618701734,2.02939404978258,-0.863036236644584));
#26275=CARTESIAN_POINT('Ctrl Pts',(100.144693117926,2.05644818337446,-0.792866236572012));
#26276=CARTESIAN_POINT('Ctrl Pts',(100.148762713041,2.08347030500095,-0.722779265571762));
#26277=CARTESIAN_POINT('Ctrl Pts',(100.152832308155,2.1069355090926,-0.651231127219556));
#26278=CARTESIAN_POINT('Ctrl Pts',(100.15690190327,2.12669204873535,-0.578616392652206));
#26279=CARTESIAN_POINT('Ctrl Pts',(100.160968878032,2.14643586743594,-0.50604841363288));
#26280=CARTESIAN_POINT('Ctrl Pts',(100.165035852795,2.16247563638747,-0.432415659130984));
#26281=CARTESIAN_POINT('Ctrl Pts',(100.169102827558,2.17470910480003,-0.358128900676611));
#26282=CARTESIAN_POINT('Ctrl Pts',(100.173168485386,2.1869386118692,-0.2838661971632));
#26283=CARTESIAN_POINT('Ctrl Pts',(100.177234143213,2.19536418859232,-0.208950379172764));
#26284=CARTESIAN_POINT('Ctrl Pts',(100.181299801041,2.19993478236944,-0.133801918226653));
#26285=CARTESIAN_POINT('Ctrl Pts',(100.185365443619,2.20450535900327,-0.0586537391457808));
#26286=CARTESIAN_POINT('Ctrl Pts',(100.189431086198,2.20522095433587,0.0167266063313277));
#26287=CARTESIAN_POINT('Ctrl Pts',(100.193496728776,2.2020825414925,0.0919156159416376));
#26288=CARTESIAN_POINT('Ctrl Pts',(100.197566376062,2.19894103727403,0.167178687647775));
#26289=CARTESIAN_POINT('Ctrl Pts',(100.201636023348,2.1919379634564,0.242249570886276));
#26290=CARTESIAN_POINT('Ctrl Pts',(100.205705670634,2.18112638065457,0.316707612179906));
#26291=CARTESIAN_POINT('Ctrl Pts',(100.209777369737,2.17030934691738,0.39120319339508));
#26292=CARTESIAN_POINT('Ctrl Pts',(100.213849068839,2.15568007182915,0.46508485016155));
#26293=CARTESIAN_POINT('Ctrl Pts',(100.217920767942,2.13734272129844,0.537942461340027));
#26294=CARTESIAN_POINT('Ctrl Pts',(100.221999535866,2.11897353554306,0.61092655962566));
#26295=CARTESIAN_POINT('Ctrl Pts',(100.22607830379,2.09688355492054,0.682882605652555));
#26296=CARTESIAN_POINT('Ctrl Pts',(100.230157071714,2.07122662006758,0.753416410972987));
#26297=CARTESIAN_POINT('Ctrl Pts',(100.233231157233,2.05188950323143,0.806576324352992));
#26298=CARTESIAN_POINT('Ctrl Pts',(100.236305242752,2.03052727456381,0.85892869107479));
#26299=CARTESIAN_POINT('Ctrl Pts',(100.239379328271,2.00722316170751,0.910313780575081));
#26300=CARTESIAN_POINT('Ctrl Pts',(100.243411081307,1.97665913634629,0.977706827817865));
#26301=CARTESIAN_POINT('Ctrl Pts',(100.247442834343,1.94263306376122,1.04369995973938));
#26302=CARTESIAN_POINT('Ctrl Pts',(100.25147458738,1.90529626114647,1.10790891198747));
#26303=CARTESIAN_POINT('Ctrl Pts',(100.25557233437,1.86734830918308,1.17316887172939));
#26304=CARTESIAN_POINT('Ctrl Pts',(100.259670081361,1.82598039289948,1.23658522006357));
#26305=CARTESIAN_POINT('Ctrl Pts',(100.263767828351,1.78140262335438,1.29777528621335));
#26306=CARTESIAN_POINT('Ctrl Pts',(100.267789135409,1.73765641361766,1.35782390450241));
#26307=CARTESIAN_POINT('Ctrl Pts',(100.271810442467,1.69081936945625,1.41572816748967));
#26308=CARTESIAN_POINT('Ctrl Pts',(100.275831749524,1.64113541697714,1.47115279394877));
#26309=CARTESIAN_POINT('Ctrl Pts',(100.279850713013,1.59148041970876,1.5265451196013));
#26310=CARTESIAN_POINT('Ctrl Pts',(100.283869676501,1.53898213005258,1.57946031247005));
#26311=CARTESIAN_POINT('Ctrl Pts',(100.28788863999,1.48392491646616,1.62959591380529));
#26312=CARTESIAN_POINT('Ctrl Pts',(100.291906624003,1.42888112105103,1.67971929643126));
#26313=CARTESIAN_POINT('Ctrl Pts',(100.295924608017,1.37128000066142,1.72706410412449));
#26314=CARTESIAN_POINT('Ctrl Pts',(100.299942592031,1.31144169603398,1.77136576626724));
#26315=CARTESIAN_POINT('Ctrl Pts',(100.304099085624,1.24954062102563,1.81719461333045));
#26316=CARTESIAN_POINT('Ctrl Pts',(100.308255579218,1.18524572013854,1.85976630705441));
#26317=CARTESIAN_POINT('Ctrl Pts',(100.312412072811,1.1189455096022,1.89883568181691));
#26318=CARTESIAN_POINT('Ctrl Pts',(100.316434556042,1.05478289775656,1.93664541285184));
#26319=CARTESIAN_POINT('Ctrl Pts',(100.320457039272,0.988742795484717,1.97117505493495));
#26320=CARTESIAN_POINT('Ctrl Pts',(100.324479522503,0.92120178309576,2.00224955358247));
#26321=CARTESIAN_POINT('Ctrl Pts',(100.328703021278,0.850285543869137,2.03487693807064));
#26322=CARTESIAN_POINT('Ctrl Pts',(100.332926520052,0.777715028177847,2.06369458611144));
#26323=CARTESIAN_POINT('Ctrl Pts',(100.337150018827,0.703946408049919,2.08855822389361));
#26324=CARTESIAN_POINT('Ctrl Pts',(100.341373517602,0.630177787921981,2.11342186167578));
#26325=CARTESIAN_POINT('Ctrl Pts',(100.345597016376,0.555211675809381,2.13433139831774));
#26326=CARTESIAN_POINT('Ctrl Pts',(100.349820515151,0.479516069206331,2.15120439274675));
#26327=CARTESIAN_POINT('',(100.349869898682,1.9893770426062,0.948680653513814));
#26328=CARTESIAN_POINT('Origin',(100.349869898682,0.,0.));
#26329=CARTESIAN_POINT('Ctrl Pts',(100.349869898682,1.9893770426062,0.948680653513815));
#26330=CARTESIAN_POINT('Ctrl Pts',(100.345705551524,2.02247380987769,0.879276951909368));
#26331=CARTESIAN_POINT('Ctrl Pts',(100.341541204365,2.05195987186717,0.808086644086603));
#26332=CARTESIAN_POINT('Ctrl Pts',(100.337376857207,2.07765243739774,0.735510944429262));
#26333=CARTESIAN_POINT('Ctrl Pts',(100.333215187647,2.10332848308289,0.662981909607237));
#26334=CARTESIAN_POINT('Ctrl Pts',(100.329053518087,2.12521573587352,0.589069675070232));
#26335=CARTESIAN_POINT('Ctrl Pts',(100.324891848527,2.1431798897202,0.514194477118237));
#26336=CARTESIAN_POINT('Ctrl Pts',(100.320730691219,2.16114183239345,0.439328495411571));
#26337=CARTESIAN_POINT('Ctrl Pts',(100.316569533911,2.17518152259502,0.363500217611781));
#26338=CARTESIAN_POINT('Ctrl Pts',(100.312408376603,2.18521504163324,0.287143207859524));
#26339=CARTESIAN_POINT('Ctrl Pts',(100.308247312157,2.19524833675862,0.210787902127007));
#26340=CARTESIAN_POINT('Ctrl Pts',(100.304086247711,2.20127557988319,0.133904330784247));
#26341=CARTESIAN_POINT('Ctrl Pts',(100.299925183266,2.20326454118416,0.0569329567170542));
#26342=CARTESIAN_POINT('Ctrl Pts',(100.295763137625,2.20525397148981,-0.0200565674943));
#26343=CARTESIAN_POINT('Ctrl Pts',(100.291601091984,2.20320321502967,-0.0971334889875312));
#26344=CARTESIAN_POINT('Ctrl Pts',(100.287439046344,2.19713218054514,-0.173856783626463));
#26345=CARTESIAN_POINT('Ctrl Pts',(100.28327494463,2.19105814693721,-0.250617979982078));
#26346=CARTESIAN_POINT('Ctrl Pts',(100.279110842917,2.18095992145872,-0.327024757020367));
#26347=CARTESIAN_POINT('Ctrl Pts',(100.274946741204,2.16690920950204,-0.40264187285382));
#26348=CARTESIAN_POINT('Ctrl Pts',(100.270776328819,2.15283720377383,-0.478373585982651));
#26349=CARTESIAN_POINT('Ctrl Pts',(100.266605916434,2.13480083408059,-0.55331280862868));
#26350=CARTESIAN_POINT('Ctrl Pts',(100.262435504048,2.11292277344509,-0.627035368585478));
#26351=CARTESIAN_POINT('Ctrl Pts',(100.258261651188,2.0910266640139,-0.700818747617783));
#26352=CARTESIAN_POINT('Ctrl Pts',(100.254087798328,2.06528269850951,-0.773383043315252));
#26353=CARTESIAN_POINT('Ctrl Pts',(100.249913945468,2.03586236903032,-0.844322458759825));
#26354=CARTESIAN_POINT('Ctrl Pts',(100.245732052254,2.00638536532792,-0.915398529243178));
#26355=CARTESIAN_POINT('Ctrl Pts',(100.24155015904,1.97321804347586,-0.984843063660913));
#26356=CARTESIAN_POINT('Ctrl Pts',(100.237368265825,1.93657857844273,-1.05227344807171));
#26357=CARTESIAN_POINT('Ctrl Pts',(100.235151904771,1.91716003301833,-1.08801086895061));
#26358=CARTESIAN_POINT('Ctrl Pts',(100.232935543717,1.89676694883971,-1.12318300253146));
#26359=CARTESIAN_POINT('Ctrl Pts',(100.230719182663,1.87543663427232,-1.15773633908128));
#26360=CARTESIAN_POINT('Ctrl Pts',(100.226681843158,1.83658117725961,-1.22067894964221));
#26361=CARTESIAN_POINT('Ctrl Pts',(100.222644503653,1.79446431510442,-1.28180751700185));
#26362=CARTESIAN_POINT('Ctrl Pts',(100.218607164148,1.74928100490527,-1.3407579818437));
#26363=CARTESIAN_POINT('Ctrl Pts',(100.214576367462,1.70417091773602,-1.39961291292253));
#26364=CARTESIAN_POINT('Ctrl Pts',(100.210545570776,1.65600453538297,-1.45629636238109));
#26365=CARTESIAN_POINT('Ctrl Pts',(100.20651477409,1.60502159852659,-1.51047067772372));
#26366=CARTESIAN_POINT('Ctrl Pts',(100.202489410823,1.55410738546927,-1.5645719673642));
#26367=CARTESIAN_POINT('Ctrl Pts',(100.198464047556,1.50038448930946,-1.6161704872544));
#26368=CARTESIAN_POINT('Ctrl Pts',(100.194438684289,1.44413353989373,-1.66496075598015));
#26369=CARTESIAN_POINT('Ctrl Pts',(100.190416300267,1.38792422282207,-1.71371491414644));
#26370=CARTESIAN_POINT('Ctrl Pts',(100.186393916244,1.32919092952845,-1.75966462457535));
#26371=CARTESIAN_POINT('Ctrl Pts',(100.182371532221,1.26825084872205,-1.80254147933295));
#26372=CARTESIAN_POINT('Ctrl Pts',(100.178350765927,1.20733527689301,-1.84540108980979));
#26373=CARTESIAN_POINT('Ctrl Pts',(100.174329999633,1.14421507644506,-1.88519001645548));
#26374=CARTESIAN_POINT('Ctrl Pts',(100.170309233339,1.07923881312582,-1.92168144712977));
#26375=CARTESIAN_POINT('Ctrl Pts',(100.166288725414,1.01426672509177,-1.95817053291498));
#26376=CARTESIAN_POINT('Ctrl Pts',(100.162268217489,0.947439236549497,-1.99136230620485));
#26377=CARTESIAN_POINT('Ctrl Pts',(100.158247709563,0.879130542096939,-2.02107533010335));
#26378=CARTESIAN_POINT('Ctrl Pts',(100.154223272099,0.810755084507366,-2.05081739473672));
#26379=CARTESIAN_POINT('Ctrl Pts',(100.150198834634,0.740895977443084,-2.07707372443632));
#26380=CARTESIAN_POINT('Ctrl Pts',(100.146174397169,0.66994767428634,-2.09971095956523));
#26381=CARTESIAN_POINT('Ctrl Pts',(100.142148026805,0.598965295331431,-2.12235906714381));
#26382=CARTESIAN_POINT('Ctrl Pts',(100.138121656441,0.526893150576154,-2.14138449574319));
#26383=CARTESIAN_POINT('Ctrl Pts',(100.134095286077,0.454138437003612,-2.15670449529738));
#26384=CARTESIAN_POINT('Ctrl Pts',(100.130061528505,0.38125023988055,-2.17205260255531));
#26385=CARTESIAN_POINT('Ctrl Pts',(100.126027770933,0.307677454727682,-2.18368162615086));
#26386=CARTESIAN_POINT('Ctrl Pts',(100.121994013361,0.233834487177226,-2.19156050169886));
#26387=CARTESIAN_POINT('Ctrl Pts',(100.118518831122,0.170216938348896,-2.19834834848393));
#26388=CARTESIAN_POINT('Ctrl Pts',(100.115043648883,0.106399111850957,-2.20235359730959));
#26389=CARTESIAN_POINT('Ctrl Pts',(100.111568466644,0.0426447683184777,
-2.20358739870582));
#26390=CARTESIAN_POINT('Ctrl Pts',(100.107492140298,-0.0321379314998587,
-2.20503462558225));
#26391=CARTESIAN_POINT('Ctrl Pts',(100.103415813953,-0.107137919792663,
-2.20267349357564));
#26392=CARTESIAN_POINT('Ctrl Pts',(100.099339487607,-0.181935437885235,
-2.19647797540552));
#26393=CARTESIAN_POINT('Ctrl Pts',(100.095269175343,-0.256622602116876,
-2.19029159790433));
#26394=CARTESIAN_POINT('Ctrl Pts',(100.091198863078,-0.331107418229155,
-2.1802821054808));
#26395=CARTESIAN_POINT('Ctrl Pts',(100.087128550814,-0.404969172531764,
-2.16647547165874));
#26396=CARTESIAN_POINT('Ctrl Pts',(100.083063058635,-0.478743459358434,
-2.15268518772469));
#26397=CARTESIAN_POINT('Ctrl Pts',(100.078997566455,-0.55189568428568,-2.13510678388212));
#26398=CARTESIAN_POINT('Ctrl Pts',(100.074932074276,-0.624010943631892,
-2.11381795389945));
#26399=CARTESIAN_POINT('Ctrl Pts',(100.070869199899,-0.696079767387687,
-2.09254283196412));
#26400=CARTESIAN_POINT('Ctrl Pts',(100.066806325523,-0.767112494745006,
-2.06756215981608));
#26401=CARTESIAN_POINT('Ctrl Pts',(100.062743451146,-0.836706396294933,
-2.03900426836217));
#26402=CARTESIAN_POINT('Ctrl Pts',(100.058681885859,-0.906277874164999,
-2.01045557847623));
#26403=CARTESIAN_POINT('Ctrl Pts',(100.054620320571,-0.974411006142448,
-1.97833213865823));
#26404=CARTESIAN_POINT('Ctrl Pts',(100.050558755283,-1.04072167636616,-1.9428109512615));
#26405=CARTESIAN_POINT('Ctrl Pts',(100.046497192096,-1.10703231230171,-1.90728978223219));
#26406=CARTESIAN_POINT('Ctrl Pts',(100.042435628908,-1.17152006911247,-1.86837109573711));
#26407=CARTESIAN_POINT('Ctrl Pts',(100.038374065721,-1.23382556728059,-1.82627776351921));
#26408=CARTESIAN_POINT('Ctrl Pts',(100.034308450996,-1.296193217134,-1.78414244188442));
#26409=CARTESIAN_POINT('Ctrl Pts',(100.030242836272,-1.35637386531743,-1.73882641771799));
#26410=CARTESIAN_POINT('Ctrl Pts',(100.026177221548,-1.41403790925473,-1.69059539547182));
#26411=CARTESIAN_POINT('Ctrl Pts',(100.022109535129,-1.47173133677111,-1.64233979638436));
#26412=CARTESIAN_POINT('Ctrl Pts',(100.01804184871,-1.52690525613829,-1.59116656516457));
#26413=CARTESIAN_POINT('Ctrl Pts',(100.013974162291,-1.57926588176533,-1.53737935288984));
#26414=CARTESIAN_POINT('Ctrl Pts',(100.00989933106,-1.63171847781615,-1.48349766441954));
#26415=CARTESIAN_POINT('Ctrl Pts',(100.005824499829,-1.68134759452345,-1.42699318221482));
#26416=CARTESIAN_POINT('Ctrl Pts',(100.001749668597,-1.72789910523482,-1.36820345056161));
#26417=CARTESIAN_POINT('Ctrl Pts',(99.9986390292732,-1.76343553646106,-1.32332462227489));
#26418=CARTESIAN_POINT('Ctrl Pts',(99.9955283899492,-1.79717931958817,-1.27711478052259));
#26419=CARTESIAN_POINT('Ctrl Pts',(99.9924177506252,-1.82903497614255,-1.22973454698451));
#26420=CARTESIAN_POINT('Ctrl Pts',(99.9883380320037,-1.87081484892997,-1.16759361680217));
#26421=CARTESIAN_POINT('Ctrl Pts',(99.9842583133821,-1.9095019130363,-1.1032056749545));
#26422=CARTESIAN_POINT('Ctrl Pts',(99.9801785947606,-1.94484752698673,-1.03691084321343));
#26423=CARTESIAN_POINT('Ctrl Pts',(99.9761047238386,-1.98014247800006,-0.97071103573465));
#26424=CARTESIAN_POINT('Ctrl Pts',(99.9720308529165,-2.01210526712443,-0.902610182078885));
#26425=CARTESIAN_POINT('Ctrl Pts',(99.9679569819944,-2.0405305570293,-0.832977218073647));
#26426=CARTESIAN_POINT('Ctrl Pts',(99.9638876981338,-2.06892384087561,-0.763422658782331));
#26427=CARTESIAN_POINT('Ctrl Pts',(99.9598184142732,-2.09378736062871,-0.692339855024764));
#26428=CARTESIAN_POINT('Ctrl Pts',(99.9557491304126,-2.1149624750193,-0.62012073764731));
#26429=CARTESIAN_POINT('Ctrl Pts',(99.9516823233637,-2.13612470095763,-0.547945577182193));
#26430=CARTESIAN_POINT('Ctrl Pts',(99.9476155163147,-2.15360284351699,-0.474635931076114));
#26431=CARTESIAN_POINT('Ctrl Pts',(99.9435487092658,-2.16728748085921,-0.400600767985965));
#26432=CARTESIAN_POINT('Ctrl Pts',(99.9394830758517,-2.18096816896875,-0.326586970612548));
#26433=CARTESIAN_POINT('Ctrl Pts',(99.9354174424376,-2.19085743937203,-0.251848539451298));
#26434=CARTESIAN_POINT('Ctrl Pts',(99.9313518090235,-2.19689689986293,-0.176805009467076));
#26435=CARTESIAN_POINT('Ctrl Pts',(99.9272860476566,-2.20293655042664,-0.101759117726364));
#26436=CARTESIAN_POINT('Ctrl Pts',(99.9232202862896,-2.20512611409972,-0.0264085823242432));
#26437=CARTESIAN_POINT('Ctrl Pts',(99.9191545249226,-2.2034591668547,0.0488231502875364));
#26438=CARTESIAN_POINT('Ctrl Pts',(99.9150845382916,-2.20179048726689,0.124133066027335));
#26439=CARTESIAN_POINT('Ctrl Pts',(99.9110145516604,-2.19625730423869,0.199323455888921));
#26440=CARTESIAN_POINT('Ctrl Pts',(99.9069445650293,-2.18690532399787,0.273972815932136));
#26441=CARTESIAN_POINT('Ctrl Pts',(99.9028724035345,-2.17754834637388,0.348662066078422));
#26442=CARTESIAN_POINT('Ctrl Pts',(99.8988002420397,-2.16436859091822,0.422809241954582));
#26443=CARTESIAN_POINT('Ctrl Pts',(99.8947280805448,-2.14746303997753,0.496002512020312));
#26444=CARTESIAN_POINT('Ctrl Pts',(99.8906486544299,-2.13052733001547,0.569326356795161));
#26445=CARTESIAN_POINT('Ctrl Pts',(99.8865692283149,-2.10985267906245,0.641692438675049));
#26446=CARTESIAN_POINT('Ctrl Pts',(99.8824898021999,-2.08558601042208,0.712704001063348));
#26447=CARTESIAN_POINT('Ctrl Pts',(99.8794155463353,-2.06729864688573,0.766218320475076));
#26448=CARTESIAN_POINT('Ctrl Pts',(99.8763412904706,-2.04697237237334,0.818963707625186));
#26449=CARTESIAN_POINT('Ctrl Pts',(99.8732670346059,-2.02468756933049,0.870779103216547));
#26450=CARTESIAN_POINT('Ctrl Pts',(99.8691983003044,-1.9951939466352,0.939356048879436));
#26451=CARTESIAN_POINT('Ctrl Pts',(99.865129566003,-1.9621542300046,1.00656781621544));
#26452=CARTESIAN_POINT('Ctrl Pts',(99.8610608317015,-1.92571655130637,1.07202227776511));
#26453=CARTESIAN_POINT('Ctrl Pts',(99.8569981432433,-1.8893330163485,1.13737947874556));
#26454=CARTESIAN_POINT('Ctrl Pts',(99.8529354547851,-1.84956177394102,1.20098414327725));
#26455=CARTESIAN_POINT('Ctrl Pts',(99.8488727663269,-1.80659876662032,1.26246461195787));
#26456=CARTESIAN_POINT('Ctrl Pts',(99.8448149078923,-1.76368683689073,1.32387198812388));
#26457=CARTESIAN_POINT('Ctrl Pts',(99.8407570494577,-1.71759095361078,1.38315979527332));
#26458=CARTESIAN_POINT('Ctrl Pts',(99.8366991910231,-1.66855182652232,1.43998291733237));
#26459=CARTESIAN_POINT('Ctrl Pts',(99.8326439525906,-1.61954436209969,1.49676935090138));
#26460=CARTESIAN_POINT('Ctrl Pts',(99.8285887141581,-1.56759773647102,1.55109389558607));
#26461=CARTESIAN_POINT('Ctrl Pts',(99.8245334757256,-1.51299380749293,1.60264335973043));
#26462=CARTESIAN_POINT('Ctrl Pts',(99.8204795373842,-1.45840738428668,1.65417629735053));
#26463=CARTESIAN_POINT('Ctrl Pts',(99.8164255990427,-1.40116569683704,1.70293559234757));
#26464=CARTESIAN_POINT('Ctrl Pts',(99.8123716607012,-1.34158729132383,1.74864505825465));
#26465=CARTESIAN_POINT('Ctrl Pts',(99.8083177042632,-1.28200861985567,1.79435472820643));
#26466=CARTESIAN_POINT('Ctrl Pts',(99.8042637478252,-1.22009359045887,1.83701425211435));
#26467=CARTESIAN_POINT('Ctrl Pts',(99.8002097913871,-1.1561923405857,1.87638889134714));
#26468=CARTESIAN_POINT('Ctrl Pts',(99.7961516982078,-1.09222588455107,1.91580370927892));
#26469=CARTESIAN_POINT('Ctrl Pts',(99.7920936050285,-1.02626956904168,1.9519266971401));
#26470=CARTESIAN_POINT('Ctrl Pts',(99.7880355118492,-0.958700267890422,
1.98456791174977));
#26471=CARTESIAN_POINT('Ctrl Pts',(99.7839753115554,-0.891095882218119,
2.01722607490502));
#26472=CARTESIAN_POINT('Ctrl Pts',(99.7799151112615,-0.82187728464676,2.04639867878928));
#26473=CARTESIAN_POINT('Ctrl Pts',(99.7758549109677,-0.75144110058728,2.07194408041052));
#26474=CARTESIAN_POINT('Ctrl Pts',(99.7717874216498,-0.680878466843862,
2.09753534209649));
#26475=CARTESIAN_POINT('Ctrl Pts',(99.7677199323318,-0.609094338978657,
2.11948625489022));
#26476=CARTESIAN_POINT('Ctrl Pts',(99.7636524430139,-0.536499815403239,
2.13770529963143));
#26477=CARTESIAN_POINT('Ctrl Pts',(99.7604737348715,-0.479767815601417,
2.15194332740185));
#26478=CARTESIAN_POINT('Ctrl Pts',(99.7572950267292,-0.422541202822639,
2.16390320940677));
#26479=CARTESIAN_POINT('Ctrl Pts',(99.7541163185868,-0.365018595209633,
2.17356330139041));
#26480=CARTESIAN_POINT('Ctrl Pts',(99.7474958281946,-0.245212732581249,
2.19368296739992));
#26481=CARTESIAN_POINT('Ctrl Pts',(99.7408753378023,-0.123701771398941,
2.20390030207451));
#26482=CARTESIAN_POINT('Ctrl Pts',(99.7342548474101,-0.00178926204916046,
2.20399927371615));
#26483=CARTESIAN_POINT('Origin',(25.4947388265965,0.,-6.40787078036307));
#26484=CARTESIAN_POINT('',(25.4947388265965,-7.48009298981943E-16,6.107959450045));
#26485=CARTESIAN_POINT('Origin',(25.4947388265965,0.,0.));
#26486=CARTESIAN_POINT('',(25.4947388265965,-7.47987577963046E-16,6.10778208446569));
#26487=CARTESIAN_POINT('Origin',(25.4947388265965,0.,0.));
#26488=CARTESIAN_POINT('Origin',(27.4542764744824,0.,0.));
#26489=CARTESIAN_POINT('',(27.7542764744824,-7.48069377062962E-16,6.10845002480549));
#26490=CARTESIAN_POINT('Origin',(27.7542764744824,0.,0.));
#26491=CARTESIAN_POINT('',(27.4541877916966,-7.84808779432149E-16,6.40845001169777));
#26492=CARTESIAN_POINT('Origin',(27.4542764744824,-7.48069377062961E-16,
6.10845002480549));
#26493=CARTESIAN_POINT('Origin',(27.4541877916966,-7.84808779432149E-16,
0.));
#26494=CARTESIAN_POINT('Origin',(26.6245076505395,0.,0.));
#26495=CARTESIAN_POINT('',(25.7946501438108,-7.8474870135113E-16,6.40795943693727));
#26496=CARTESIAN_POINT('',(26.6245076505395,-7.84778743602106E-16,6.40820475053297));
#26497=CARTESIAN_POINT('Origin',(25.7946501438108,-7.8474870135113E-16,
0.));
#26498=CARTESIAN_POINT('Origin',(25.7947388265966,0.,0.));
#26499=CARTESIAN_POINT('Origin',(25.7947388265966,-7.48009298981944E-16,
6.107959450045));
#26500=CARTESIAN_POINT('Origin',(27.7542764744824,0.,-6.40853872070288));
#26501=CARTESIAN_POINT('',(27.7542764744824,-7.4809109808186E-16,6.1086273903848));
#26502=CARTESIAN_POINT('Origin',(27.7542764744824,0.,0.));
#26503=CARTESIAN_POINT('Ctrl Pts',(90.0988178106407,1.30236646373779,-1.19759169991716));
#26504=CARTESIAN_POINT('Ctrl Pts',(90.1385586184198,1.70110773626567,-0.764007006172047));
#26505=CARTESIAN_POINT('Ctrl Pts',(90.2180163315385,2.02395293608162,0.525231536151233));
#26506=CARTESIAN_POINT('Ctrl Pts',(90.3371909499971,0.652775565002029,1.98853514061584));
#26507=CARTESIAN_POINT('Ctrl Pts',(90.4563416660163,-1.31672770966033,1.62464706040724));
#26508=CARTESIAN_POINT('Ctrl Pts',(90.5754923820352,-2.07940182116321,-0.225715520989952));
#26509=CARTESIAN_POINT('Ctrl Pts',(90.6946430980545,-0.936716819385667,
-1.87038353007312));
#26510=CARTESIAN_POINT('Ctrl Pts',(90.8137938140736,1.06439707893563,-1.80053599719708));
#26511=CARTESIAN_POINT('Ctrl Pts',(90.9329445300927,2.09011102819176,-0.0810387888271981));
#26512=CARTESIAN_POINT('Ctrl Pts',(91.052095246112,1.20054819198944,1.71286342585472));
#26513=CARTESIAN_POINT('Ctrl Pts',(91.171245962131,-0.789155321291253,1.93709542934556));
#26514=CARTESIAN_POINT('Ctrl Pts',(91.2903966781501,-2.05570548030766,0.386289109614587));
#26515=CARTESIAN_POINT('Ctrl Pts',(91.4095473941693,-1.43849345547043,-1.51851496410962));
#26516=CARTESIAN_POINT('Ctrl Pts',(91.5286981101884,0.496895874116886,-2.03180509569764));
#26517=CARTESIAN_POINT('Ctrl Pts',(91.6478488262076,1.97694974251289,-0.683237063999725));
#26518=CARTESIAN_POINT('Ctrl Pts',(91.7669995422267,1.6454082772736,1.29142367419714));
#26519=CARTESIAN_POINT('Ctrl Pts',(91.8861502582457,-0.193917899418074,
2.0826756182632));
#26520=CARTESIAN_POINT('Ctrl Pts',(92.005300974265,-1.85554561362532,0.965449717325565));
#26521=CARTESIAN_POINT('Ctrl Pts',(92.1244516902841,-1.81682754149423,-1.03647495873235));
#26522=CARTESIAN_POINT('Ctrl Pts',(92.2436024063033,-0.113243288550902,
-2.08861639028052));
#26523=CARTESIAN_POINT('Ctrl Pts',(92.3627531223225,1.69411245684142,-1.22683558804683));
#26524=CARTESIAN_POINT('Ctrl Pts',(92.4819038383415,1.94905310597792,0.759167013834017));
#26525=CARTESIAN_POINT('Ctrl Pts',(92.6010545543606,0.417961509270532,2.04950011481713));
#26526=CARTESIAN_POINT('Ctrl Pts',(92.7202052703798,-1.49613285327444,1.46175546640634));
#26527=CARTESIAN_POINT('Ctrl Pts',(92.8393559863988,-2.03923249641387,-0.465481880699497));
#26528=CARTESIAN_POINT('Ctrl Pts',(92.958506702418,-0.713663204520452,-1.96617074130422));
#26529=CARTESIAN_POINT('Ctrl Pts',(93.0776574184373,1.26587774694564,-1.66514146098521));
#26530=CARTESIAN_POINT('Ctrl Pts',(93.1968081344563,2.08542030441444,0.161755088931124));
#26531=CARTESIAN_POINT('Ctrl Pts',(93.3159588504756,0.993969316150796,1.84042591624436));
#26532=CARTESIAN_POINT('Ctrl Pts',(93.4351095664945,-1.00831434394197,1.83260599657131));
#26533=CARTESIAN_POINT('Ctrl Pts',(93.5542602825138,-2.0866201376949,0.145461183012646));
#26534=CARTESIAN_POINT('Ctrl Pts',(93.6734109985329,-1.25283290778611,-1.67497828640997));
#26535=CARTESIAN_POINT('Ctrl Pts',(93.7925617145521,0.728998961157423,-1.96053642389964));
#26536=CARTESIAN_POINT('Ctrl Pts',(93.9117124305713,2.04280611266453,-0.449539476415141));
#26537=CARTESIAN_POINT('Ctrl Pts',(94.0308631465901,1.48466961417535,1.47339699047405));
#26538=CARTESIAN_POINT('Ctrl Pts',(94.1500138626095,-0.433957162547644,
2.04617294867045));
#26539=CARTESIAN_POINT('Ctrl Pts',(94.2691645786286,-1.95492341252519,0.743920026586493));
#26540=CARTESIAN_POINT('Ctrl Pts',(94.3883152946477,-1.68447811070772,-1.24003066467813));
#26541=CARTESIAN_POINT('Ctrl Pts',(94.5074660106668,0.129553772013031,-2.0876681668678));
#26542=CARTESIAN_POINT('Ctrl Pts',(94.6266167266861,1.82486789716038,-1.0222522744945));
#26543=CARTESIAN_POINT('Ctrl Pts',(94.7457674427052,1.84794800509362,0.97991363153406));
#26544=CARTESIAN_POINT('Ctrl Pts',(94.8649181587243,0.177644432504533,2.08412691801531));
#26545=CARTESIAN_POINT('Ctrl Pts',(94.9840688747434,-1.65544520447039,1.27853186498882));
#26546=CARTESIAN_POINT('Ctrl Pts',(95.1032195907626,-1.97155282381159,-0.698657296330842));
#26547=CARTESIAN_POINT('Ctrl Pts',(95.2223703067817,-0.48101038161002,-2.03562559612007));
#26548=CARTESIAN_POINT('Ctrl Pts',(95.3415210228009,1.4503102254182,-1.50723017646382));
#26549=CARTESIAN_POINT('Ctrl Pts',(95.4606717388199,2.05262608737329,0.402329094436875));
#26550=CARTESIAN_POINT('Ctrl Pts',(95.5798224548391,0.773999677688958,1.94321050165266));
#26551=CARTESIAN_POINT('Ctrl Pts',(95.6989731708583,-1.21388825846436,1.70341358769916));
#26552=CARTESIAN_POINT('Ctrl Pts',(95.8181238868774,-2.0894188332659,-0.0973216008372093));
#26553=CARTESIAN_POINT('Ctrl Pts',(95.9372746028964,-1.05029177469469,-1.80887527010699));
#26554=CARTESIAN_POINT('Ctrl Pts',(96.0564253189157,0.951279544295426,-1.86284990898372));
#26555=CARTESIAN_POINT('Ctrl Pts',(96.1755760349347,2.0811373456516,-0.209785374442143));
#26556=CARTESIAN_POINT('Ctrl Pts',(96.294726750954,1.30392632887128,1.63551786406429));
#26557=CARTESIAN_POINT('Ctrl Pts',(96.4138774669731,-0.668149240282063,
1.98209968152566));
#26558=CARTESIAN_POINT('Ctrl Pts',(96.5330281829921,-2.02796027789557,0.512366730060481));
#26559=CARTESIAN_POINT('Ctrl Pts',(96.6521788990114,-1.52943177897067,-1.42687805655579));
#26560=CARTESIAN_POINT('Ctrl Pts',(96.7713296150304,0.370605208206405,-2.05859037557912));
#26561=CARTESIAN_POINT('Ctrl Pts',(96.8904803310495,1.93103479854338,-0.803894994145272));
#26562=CARTESIAN_POINT('Ctrl Pts',(97.0096310470688,1.72194338215499,1.18745675437928));
#26563=CARTESIAN_POINT('Ctrl Pts',(97.1287817630879,-0.065066251703002,
2.0906718866246));
#26564=CARTESIAN_POINT('Ctrl Pts',(97.247932479107,-1.7924518438776,1.07808113898674));
#26565=CARTESIAN_POINT('Ctrl Pts',(97.3670831951263,-1.87730815926342,-0.922418901837522));
#26566=CARTESIAN_POINT('Ctrl Pts',(97.4862339111451,-0.241876354077899,
-2.07765213228422));
#26567=CARTESIAN_POINT('Ctrl Pts',(97.6053846271646,1.61520101083011,-1.32901025214378));
#26568=CARTESIAN_POINT('Ctrl Pts',(97.7245353431835,1.9921744856802,0.637482059999133));
#26569=CARTESIAN_POINT('Ctrl Pts',(97.8436860592028,0.54360105305752,2.01981198109672));
#26570=CARTESIAN_POINT('Ctrl Pts',(97.9628367752219,-1.4031060626124,1.55126913908458));
#26571=CARTESIAN_POINT('Ctrl Pts',(98.081987491241,-2.06406439651977,-0.338793068912289));
#26572=CARTESIAN_POINT('Ctrl Pts',(98.2011382072602,-0.833598848803122,
-1.91839918354454));
#26573=CARTESIAN_POINT('Ctrl Pts',(98.3202889232793,1.16074243271934,-1.74006311968733));
#26574=CARTESIAN_POINT('Ctrl Pts',(98.4394396392984,2.09142705758357,0.032795483461962));
#26575=CARTESIAN_POINT('Ctrl Pts',(98.5585903553176,1.10561369120534,1.77560137656009));
#26576=CARTESIAN_POINT('Ctrl Pts',(98.6777410713367,-0.893338462267605,
1.891319617894));
#26577=CARTESIAN_POINT('Ctrl Pts',(98.7968917873559,-2.07367233759831,0.27390912055697));
#26578=CARTESIAN_POINT('Ctrl Pts',(98.9160425033749,-1.35377720344853,-1.59449827219737));
#26579=CARTESIAN_POINT('Ctrl Pts',(99.0351932193941,0.606662148098891,-2.00177724927629));
#26580=CARTESIAN_POINT('Ctrl Pts',(99.1543439354132,2.01118446085511,-0.574701107001492));
#26581=CARTESIAN_POINT('Ctrl Pts',(99.2734946514324,1.57273344194911,1.37899033502367));
#26582=CARTESIAN_POINT('Ctrl Pts',(99.3926453674515,-0.306893054534305,
2.06906590760142));
#26583=CARTESIAN_POINT('Ctrl Pts',(99.5117960834707,-1.90532100320877,0.863066202672188));
#26584=CARTESIAN_POINT('Ctrl Pts',(99.6309467994897,-1.75773992851836,-1.13367603950222));
#26585=CARTESIAN_POINT('Ctrl Pts',(99.750097515509,0.000460101095811506,
-2.09183477779575));
#26586=CARTESIAN_POINT('Ctrl Pts',(99.869248231528,1.75844121890259,-1.13258284903887));
#26587=CARTESIAN_POINT('Ctrl Pts',(99.9883989475472,1.90465462099256,0.863446991429658));
#26588=CARTESIAN_POINT('Ctrl Pts',(100.107549663566,0.306334449084961,2.07039782385695));
#26589=CARTESIAN_POINT('Ctrl Pts',(100.226715227927,-1.57465064547374,1.37565407054423));
#26590=CARTESIAN_POINT('Ctrl Pts',(100.30616388695,-1.86309197916195,0.0785106641831038));
#26591=CARTESIAN_POINT('Ctrl Pts',(100.345895640631,-1.70077331743764,-0.487600721360894));
#26592=CARTESIAN_POINT('Ctrl Pts',(90.1836630036807,1.41054030214643,-1.29706300437212));
#26593=CARTESIAN_POINT('Ctrl Pts',(90.2234038114599,1.84240080430918,-0.827465005690515));
#26594=CARTESIAN_POINT('Ctrl Pts',(90.3028615245785,2.19206134792296,0.568856977147052));
#26595=CARTESIAN_POINT('Ctrl Pts',(90.422036143037,0.706994742516013,2.15370176994804));
#26596=CARTESIAN_POINT('Ctrl Pts',(90.5411868590562,-1.42609438521506,1.75958934698854));
#26597=CARTESIAN_POINT('Ctrl Pts',(90.6603375750753,-2.25211578674213,-0.244463327366812));
#26598=CARTESIAN_POINT('Ctrl Pts',(90.7794882910944,-1.01452000049959,-2.02573655195885));
#26599=CARTESIAN_POINT('Ctrl Pts',(90.8986390071135,1.15280531181421,-1.95008752162037));
#26600=CARTESIAN_POINT('Ctrl Pts',(91.0177897231328,2.26371449458543,-0.0877698258214138));
#26601=CARTESIAN_POINT('Ctrl Pts',(91.1369404391518,1.30026506104129,1.85513291497586));
#26602=CARTESIAN_POINT('Ctrl Pts',(91.2560911551711,-0.854702125959167,
2.09798950470033));
#26603=CARTESIAN_POINT('Ctrl Pts',(91.3752418711901,-2.22645124091666,0.418374069482609));
#26604=CARTESIAN_POINT('Ctrl Pts',(91.4943925872093,-1.55797392654873,-1.64464197745212));
#26605=CARTESIAN_POINT('Ctrl Pts',(91.6135433032284,0.538167770690726,-2.20056570357529));
#26606=CARTESIAN_POINT('Ctrl Pts',(91.7326940192475,2.14115409508415,-0.739986356778505));
#26607=CARTESIAN_POINT('Ctrl Pts',(91.8518447352668,1.78207497904909,1.39868861055673));
#26608=CARTESIAN_POINT('Ctrl Pts',(91.9709954512857,-0.210024612927857,
2.25566150361919));
#26609=CARTESIAN_POINT('Ctrl Pts',(92.090146167305,-2.00966620637468,1.04563943705615));
#26610=CARTESIAN_POINT('Ctrl Pts',(92.209296883324,-1.96773223257935,-1.1225639957448));
#26611=CARTESIAN_POINT('Ctrl Pts',(92.3284475993433,-0.122649213486525,
-2.26209571287564));
#26612=CARTESIAN_POINT('Ctrl Pts',(92.4475983153624,1.8348245008436,-1.32873587368108));
#26613=CARTESIAN_POINT('Ctrl Pts',(92.5667490313815,2.11094037934247,0.822223006264858));
#26614=CARTESIAN_POINT('Ctrl Pts',(92.6858997474007,0.452677161142528,2.21973046119938));
#26615=CARTESIAN_POINT('Ctrl Pts',(92.8050504634197,-1.62040082086588,1.58316806725156));
#26616=CARTESIAN_POINT('Ctrl Pts',(92.924201179439,-2.20861002008845,-0.504144548348667));
#26617=CARTESIAN_POINT('Ctrl Pts',(93.043351895458,-0.772939675708481,-2.12947979599473));
#26618=CARTESIAN_POINT('Ctrl Pts',(93.1625026114772,1.37102085271187,-1.80344719008944));
#26619=CARTESIAN_POINT('Ctrl Pts',(93.2816533274963,2.25863416188464,0.175190377184455));
#26620=CARTESIAN_POINT('Ctrl Pts',(93.4008040435155,1.07652785799153,1.99329067528883));
#26621=CARTESIAN_POINT('Ctrl Pts',(93.5199547595345,-1.09206437585973,1.98482123741135));
#26622=CARTESIAN_POINT('Ctrl Pts',(93.6391054755538,-2.25993365265399,0.157543108449209));
#26623=CARTESIAN_POINT('Ctrl Pts',(93.7582561915729,-1.35689251642417,-1.81410105679525));
#26624=CARTESIAN_POINT('Ctrl Pts',(93.8774069075921,0.789549211812653,-2.1233774953017));
#26625=CARTESIAN_POINT('Ctrl Pts',(93.996557623611,2.21248045892906,-0.486877976778926));
#26626=CARTESIAN_POINT('Ctrl Pts',(94.1157083396304,1.60798545146521,1.5957765298718));
#26627=CARTESIAN_POINT('Ctrl Pts',(94.2348590556494,-0.470001404536919,
2.21612694247214));
#26628=CARTESIAN_POINT('Ctrl Pts',(94.3540097716686,-2.11729827030588,0.805709612686535));
#26629=CARTESIAN_POINT('Ctrl Pts',(94.4731604876876,-1.8243899312468,-1.34302692608189));
#26630=CARTESIAN_POINT('Ctrl Pts',(94.5923112037068,0.140314436687032,-2.26106873055054));
#26631=CARTESIAN_POINT('Ctrl Pts',(94.711461919726,1.97644041574166,-1.10715998321782));
#26632=CARTESIAN_POINT('Ctrl Pts',(94.8306126357451,2.00143754467901,1.06130471598179));
#26633=CARTESIAN_POINT('Ctrl Pts',(94.9497633517643,0.192399480849997,2.25723334752628));
#26634=CARTESIAN_POINT('Ctrl Pts',(95.0689140677833,-1.79294556786947,1.38472601480337));
#26635=CARTESIAN_POINT('Ctrl Pts',(95.1880647838026,-2.13530891129945,-0.756687385081276));
#26636=CARTESIAN_POINT('Ctrl Pts',(95.3072154998216,-0.520962837959247,
-2.20470353265046));
#26637=CARTESIAN_POINT('Ctrl Pts',(95.4263662158408,1.57077219087492,-1.63241988158377));
#26638=CARTESIAN_POINT('Ctrl Pts',(95.5455169318599,2.22311607530774,0.435746326575808));
#26639=CARTESIAN_POINT('Ctrl Pts',(95.6646676478791,0.838287662978745,2.10461249153227));
#26640=CARTESIAN_POINT('Ctrl Pts',(95.7838183638982,-1.31471314606197,1.84489817848784));
#26641=CARTESIAN_POINT('Ctrl Pts',(95.9029690799174,-2.26296480633173,-0.105405079194289));
#26642=CARTESIAN_POINT('Ctrl Pts',(96.0221197959364,-1.13752842880178,-1.95911944992743));
#26643=CARTESIAN_POINT('Ctrl Pts',(96.1412705119557,1.0302922972887,-2.01757719246707));
#26644=CARTESIAN_POINT('Ctrl Pts',(96.2604212279747,2.25399546293495,-0.227210031654438));
#26645=CARTESIAN_POINT('Ctrl Pts',(96.3795719439939,1.41222972881548,1.77136307358693));
#26646=CARTESIAN_POINT('Ctrl Pts',(96.498722660013,-0.723645346764778,2.14673178518397));
#26647=CARTESIAN_POINT('Ctrl Pts',(96.6178733760322,-2.19640153733235,0.554923627375294));
#26648=CARTESIAN_POINT('Ctrl Pts',(96.7370240920512,-1.65646553691972,-1.54539375902228));
#26649=CARTESIAN_POINT('Ctrl Pts',(96.8561748080704,0.401387471894955,-2.22957575399431));
#26650=CARTESIAN_POINT('Ctrl Pts',(96.9753255240896,2.0914254812546,-0.870666067891006));
#26651=CARTESIAN_POINT('Ctrl Pts',(97.0944762401087,1.86496704742619,1.28608625586138));
#26652=CARTESIAN_POINT('Ctrl Pts',(97.2136269561279,-0.0704706185947552,
2.26432193760961));
#26653=CARTESIAN_POINT('Ctrl Pts',(97.332777672147,-1.94133190299583,1.16762596232738));
#26654=CARTESIAN_POINT('Ctrl Pts',(97.4519283881662,-2.03323633702113,-0.999034505825096));
#26655=CARTESIAN_POINT('Ctrl Pts',(97.5710791041852,-0.261966470315861,
-2.25022076967224));
#26656=CARTESIAN_POINT('Ctrl Pts',(97.6902298202045,1.74935871375617,-1.43939710888626));
#26657=CARTESIAN_POINT('Ctrl Pts',(97.8093805362235,2.15764339700129,0.69043096744322));
#26658=CARTESIAN_POINT('Ctrl Pts',(97.9285312522427,0.588752255971226,2.18757644750652));
#26659=CARTESIAN_POINT('Ctrl Pts',(98.0476819682618,-1.51964727640531,1.68011669609097));
#26660=CARTESIAN_POINT('Ctrl Pts',(98.166832684281,-2.23550444408775,-0.366933033899782));
#26661=CARTESIAN_POINT('Ctrl Pts',(98.2859834003001,-0.902837108293679,
-2.07774035906009));
#26662=CARTESIAN_POINT('Ctrl Pts',(98.4051341163192,1.25715305741451,-1.88459180033968));
#26663=CARTESIAN_POINT('Ctrl Pts',(98.5242848323384,2.26513983265089,0.0355194581859003));
#26664=CARTESIAN_POINT('Ctrl Pts',(98.6434355483575,1.1974453531107,1.92308184517942));
#26665=CARTESIAN_POINT('Ctrl Pts',(98.7625862643768,-0.967538661022872,
2.04841157965873));
#26666=CARTESIAN_POINT('Ctrl Pts',(98.8817369803958,-2.24591041544012,0.296659860667986));
#26667=CARTESIAN_POINT('Ctrl Pts',(99.000887696415,-1.46622118947291,-1.72693641709899));
#26668=CARTESIAN_POINT('Ctrl Pts',(99.1200384124339,0.657051170700659,-2.16804376083236));
#26669=CARTESIAN_POINT('Ctrl Pts',(99.2391891284533,2.17823233020374,-0.622435463200776));
#26670=CARTESIAN_POINT('Ctrl Pts',(99.3583398444722,1.70336381208397,1.49352850981649));
#26671=CARTESIAN_POINT('Ctrl Pts',(99.4774905604915,-0.33238342196486,2.24092137791455));
#26672=CARTESIAN_POINT('Ctrl Pts',(99.5966412765106,-2.06357591229645,0.934752004282814));
#26673=CARTESIAN_POINT('Ctrl Pts',(99.7157919925298,-1.90373683513884,-1.22783854454161));
#26674=CARTESIAN_POINT('Ctrl Pts',(99.8349427085489,0.00049831683842665,
-2.26558141787846));
#26675=CARTESIAN_POINT('Ctrl Pts',(99.9540934245681,1.90449637431464,-1.22665455428283));
#26676=CARTESIAN_POINT('Ctrl Pts',(100.073244140587,2.06285418074182,0.935164421143912));
#26677=CARTESIAN_POINT('Ctrl Pts',(100.192394856606,0.331778419055773,2.24236392239785));
#26678=CARTESIAN_POINT('Ctrl Pts',(100.311560420967,-1.70544025747331,1.48991513705402));
#26679=CARTESIAN_POINT('Ctrl Pts',(100.39100907999,-2.01783936886045,0.0850317165421618));
#26680=CARTESIAN_POINT('Ctrl Pts',(100.430740833671,-1.84203860883819,-0.528100567686047));
#26681=CARTESIAN_POINT('Ctrl Pts',(90.2685081967207,1.51871414055506,-1.39653430882706));
#26682=CARTESIAN_POINT('Ctrl Pts',(90.3082490044998,1.98369387235267,-0.890923005208982));
#26683=CARTESIAN_POINT('Ctrl Pts',(90.3877067176185,2.36016975976431,0.612482418142867));
#26684=CARTESIAN_POINT('Ctrl Pts',(90.5068813360772,0.761213920029996,2.31886839928025));
#26685=CARTESIAN_POINT('Ctrl Pts',(90.626032052096,-1.53546106076978,1.89453163356984));
#26686=CARTESIAN_POINT('Ctrl Pts',(90.7451827681155,-2.42482975232106,-0.263211133743666));
#26687=CARTESIAN_POINT('Ctrl Pts',(90.8643334841343,-1.09232318161353,-2.18108957384459));
#26688=CARTESIAN_POINT('Ctrl Pts',(90.9834842001537,1.24121354469281,-2.09963904604366));
#26689=CARTESIAN_POINT('Ctrl Pts',(91.1026349161728,2.43731796097908,-0.0945008628156303));
#26690=CARTESIAN_POINT('Ctrl Pts',(91.2217856321918,1.39998193009314,1.99740240409698));
#26691=CARTESIAN_POINT('Ctrl Pts',(91.3409363482112,-0.920248930627077,
2.2588835800551));
#26692=CARTESIAN_POINT('Ctrl Pts',(91.4600870642302,-2.39719700152565,0.450459029350631));
#26693=CARTESIAN_POINT('Ctrl Pts',(91.5792377802492,-1.67745439762702,-1.77076899079462));
#26694=CARTESIAN_POINT('Ctrl Pts',(91.6983884962685,0.57943966726456,-2.36932631145295));
#26695=CARTESIAN_POINT('Ctrl Pts',(91.8175392122875,2.30535844765541,-0.796735649557284));
#26696=CARTESIAN_POINT('Ctrl Pts',(91.9366899283068,1.91874168082458,1.5059535469163));
#26697=CARTESIAN_POINT('Ctrl Pts',(92.0558406443258,-0.22613132643764,2.42864738897517));
#26698=CARTESIAN_POINT('Ctrl Pts',(92.174991360345,-2.16378679912404,1.12582915678676));
#26699=CARTESIAN_POINT('Ctrl Pts',(92.2941420763643,-2.11863692366447,-1.20865303275725));
#26700=CARTESIAN_POINT('Ctrl Pts',(92.4132927923833,-0.132055138422147,
-2.43557503547077));
#26701=CARTESIAN_POINT('Ctrl Pts',(92.5324435084023,1.97553654484576,-1.43063615931535));
#26702=CARTESIAN_POINT('Ctrl Pts',(92.6515942244216,2.272827652707,0.8852789986957));
#26703=CARTESIAN_POINT('Ctrl Pts',(92.7707449404406,0.487392813014522,2.38996080758163));
#26704=CARTESIAN_POINT('Ctrl Pts',(92.88989565646,-1.74466878845731,1.70458066809679));
#26705=CARTESIAN_POINT('Ctrl Pts',(93.0090463724789,-2.37798754376304,-0.542807215997835));
#26706=CARTESIAN_POINT('Ctrl Pts',(93.128197088498,-0.832216146896508,-2.29278885068523));
#26707=CARTESIAN_POINT('Ctrl Pts',(93.2473478045172,1.4761639584781,-1.94175291919367));
#26708=CARTESIAN_POINT('Ctrl Pts',(93.3664985205364,2.43184801935483,0.188625665437788));
#26709=CARTESIAN_POINT('Ctrl Pts',(93.4856492365556,1.15908639983226,2.14615543433331));
#26710=CARTESIAN_POINT('Ctrl Pts',(93.6047999525747,-1.17581440777752,2.13703647825138));
#26711=CARTESIAN_POINT('Ctrl Pts',(93.7239506685937,-2.43324716761307,0.169625033885773));
#26712=CARTESIAN_POINT('Ctrl Pts',(93.8431013846129,-1.46095212506224,-1.95322382718053));
#26713=CARTESIAN_POINT('Ctrl Pts',(93.9622521006321,0.850099462467886,-2.28621856670378));
#26714=CARTESIAN_POINT('Ctrl Pts',(94.081402816651,2.38215480519359,-0.524216477142713));
#26715=CARTESIAN_POINT('Ctrl Pts',(94.2005535326705,1.73130128875504,1.71815606926955));
#26716=CARTESIAN_POINT('Ctrl Pts',(94.3197042486894,-0.506045646526193,
2.38608093627382));
#26717=CARTESIAN_POINT('Ctrl Pts',(94.4388549647086,-2.27967312808658,0.867499198786582));
#26718=CARTESIAN_POINT('Ctrl Pts',(94.5580056807278,-1.96430175178589,-1.44602318748566));
#26719=CARTESIAN_POINT('Ctrl Pts',(94.6771563967469,0.151075101361031,-2.43446929423327));
#26720=CARTESIAN_POINT('Ctrl Pts',(94.796307112766,2.12801293432294,-1.19206769194113));
#26721=CARTESIAN_POINT('Ctrl Pts',(94.9154578287851,2.15492708426441,1.14269580042952));
#26722=CARTESIAN_POINT('Ctrl Pts',(95.0346085448042,0.207154529195459,2.43033977703725));
#26723=CARTESIAN_POINT('Ctrl Pts',(95.1537592608234,-1.93044593126855,1.49092016461792));
#26724=CARTESIAN_POINT('Ctrl Pts',(95.2729099768426,-2.29906499878732,-0.814717473831705));
#26725=CARTESIAN_POINT('Ctrl Pts',(95.3920606928618,-0.560915294308474,
-2.37378146918088));
#26726=CARTESIAN_POINT('Ctrl Pts',(95.5112114088808,1.69123415633164,-1.75760958670372));
#26727=CARTESIAN_POINT('Ctrl Pts',(95.6303621249,2.39360606324219,0.469163558714741));
#26728=CARTESIAN_POINT('Ctrl Pts',(95.749512840919,0.90257564826853,2.26601448141187));
#26729=CARTESIAN_POINT('Ctrl Pts',(95.8686635569383,-1.41553803365958,1.98638276927655));
#26730=CARTESIAN_POINT('Ctrl Pts',(95.9878142729574,-2.43651077939756,-0.113488557551372));
#26731=CARTESIAN_POINT('Ctrl Pts',(96.1069649889766,-1.22476508290887,-2.10936362974787));
#26732=CARTESIAN_POINT('Ctrl Pts',(96.2261157049957,1.10930505028198,-2.17230447595042));
#26733=CARTESIAN_POINT('Ctrl Pts',(96.3452664210148,2.42685358021832,-0.244634688866736));
#26734=CARTESIAN_POINT('Ctrl Pts',(96.4644171370341,1.52053312875968,1.90720828310958));
#26735=CARTESIAN_POINT('Ctrl Pts',(96.5835678530531,-0.77914145324749,2.31136388884227));
#26736=CARTESIAN_POINT('Ctrl Pts',(96.7027185690724,-2.36484279676913,0.597480524690107));
#26737=CARTESIAN_POINT('Ctrl Pts',(96.8218692850914,-1.78349929486876,-1.66390946148877));
#26738=CARTESIAN_POINT('Ctrl Pts',(96.9410200011106,0.432169735583501,-2.40056113240953));
#26739=CARTESIAN_POINT('Ctrl Pts',(97.0601707171294,2.2518161639658,-0.937437141636736));
#26740=CARTESIAN_POINT('Ctrl Pts',(97.1793214331488,2.00799071269739,1.38471575734347));
#26741=CARTESIAN_POINT('Ctrl Pts',(97.2984721491679,-0.0758749854865103,
2.4379719885946));
#26742=CARTESIAN_POINT('Ctrl Pts',(97.417622865187,-2.09021196211405,1.25717078566802));
#26743=CARTESIAN_POINT('Ctrl Pts',(97.5367735812062,-2.18916451477885,-1.07565010981266));
#26744=CARTESIAN_POINT('Ctrl Pts',(97.6559242972254,-0.282056586553822,
-2.42278940706025));
#26745=CARTESIAN_POINT('Ctrl Pts',(97.7750750132444,1.88351641668224,-1.54978396562876));
#26746=CARTESIAN_POINT('Ctrl Pts',(97.8942257292636,2.32311230832238,0.743379874887306));
#26747=CARTESIAN_POINT('Ctrl Pts',(98.0133764452828,0.633903458884932,2.35534091391632));
#26748=CARTESIAN_POINT('Ctrl Pts',(98.1325271613019,-1.63618849019823,1.80896425309736));
#26749=CARTESIAN_POINT('Ctrl Pts',(98.2516778773212,-2.40694449165574,-0.395072998887273));
#26750=CARTESIAN_POINT('Ctrl Pts',(98.3708285933402,-0.972075367784237,
-2.23708153457564));
#26751=CARTESIAN_POINT('Ctrl Pts',(98.4899793093593,1.3535636821097,-2.02912048099205));
#26752=CARTESIAN_POINT('Ctrl Pts',(98.6091300253786,2.4388526077182,0.0382434329098399));
#26753=CARTESIAN_POINT('Ctrl Pts',(98.7282807413975,1.28927701501606,2.07056231379875));
#26754=CARTESIAN_POINT('Ctrl Pts',(98.8474314574167,-1.04173885977815,2.20550354142346));
#26755=CARTESIAN_POINT('Ctrl Pts',(98.966582173436,-2.41814849328193,0.319410600779003));
#26756=CARTESIAN_POINT('Ctrl Pts',(99.0857328894549,-1.5786651754973,-1.85937456200061));
#26757=CARTESIAN_POINT('Ctrl Pts',(99.2048836054743,0.707440193302429,-2.33431027238844));
#26758=CARTESIAN_POINT('Ctrl Pts',(99.3240343214933,2.34528019955236,-0.670169819400066));
#26759=CARTESIAN_POINT('Ctrl Pts',(99.4431850375124,1.8339941822188,1.60806668460931));
#26760=CARTESIAN_POINT('Ctrl Pts',(99.5623357535317,-0.357873789395414,
2.41277684822769));
#26761=CARTESIAN_POINT('Ctrl Pts',(99.6814864695508,-2.22183082138415,1.00643780589344));
#26762=CARTESIAN_POINT('Ctrl Pts',(99.8006371855698,-2.04973374175933,-1.322001049581));
#26763=CARTESIAN_POINT('Ctrl Pts',(99.9197879015891,0.000536532581040912,
-2.43932805796117));
#26764=CARTESIAN_POINT('Ctrl Pts',(100.038938617608,2.05055152972668,-1.32072625952678));
#26765=CARTESIAN_POINT('Ctrl Pts',(100.158089333627,2.22105374049109,1.00688185085817));
#26766=CARTESIAN_POINT('Ctrl Pts',(100.277240049646,0.357222389026584,2.41433002093876));
#26767=CARTESIAN_POINT('Ctrl Pts',(100.396405614007,-1.83622986947288,1.6041762035638));
#26768=CARTESIAN_POINT('Ctrl Pts',(100.47585427303,-2.17258675855896,0.0915527689012232));
#26769=CARTESIAN_POINT('Ctrl Pts',(100.515586026711,-1.98330390023875,-0.568600414011198));
#26770=CARTESIAN_POINT('Ctrl Pts',(90.3533533897608,1.6268879789637,-1.49600561328201));
#26771=CARTESIAN_POINT('Ctrl Pts',(90.3930941975399,2.12498694039619,-0.954381004727451));
#26772=CARTESIAN_POINT('Ctrl Pts',(90.4725519106586,2.52827817160566,0.656107859138686));
#26773=CARTESIAN_POINT('Ctrl Pts',(90.5917265291171,0.81543309754398,2.48403502861246));
#26774=CARTESIAN_POINT('Ctrl Pts',(90.7108772451363,-1.64482773632451,2.02947392015113));
#26775=CARTESIAN_POINT('Ctrl Pts',(90.8300279611553,-2.59754371789998,-0.281958940120525));
#26776=CARTESIAN_POINT('Ctrl Pts',(90.9491786771745,-1.17012636272745,-2.33644259573031));
#26777=CARTESIAN_POINT('Ctrl Pts',(91.0683293931936,1.3296217775714,-2.24919057046694));
#26778=CARTESIAN_POINT('Ctrl Pts',(91.1874801092128,2.61092142737275,-0.101231899809847));
#26779=CARTESIAN_POINT('Ctrl Pts',(91.306630825232,1.499698799145,2.1396718932181));
#26780=CARTESIAN_POINT('Ctrl Pts',(91.4257815412509,-0.985795735294989,
2.41977765540987));
#26781=CARTESIAN_POINT('Ctrl Pts',(91.5449322572702,-2.56794276213465,0.482543989218656));
#26782=CARTESIAN_POINT('Ctrl Pts',(91.6640829732894,-1.79693486870532,-1.89689600413712));
#26783=CARTESIAN_POINT('Ctrl Pts',(91.7832336893085,0.620711563838398,-2.53808691933059));
#26784=CARTESIAN_POINT('Ctrl Pts',(91.9023844053276,2.46956280022668,-0.853484942336065));
#26785=CARTESIAN_POINT('Ctrl Pts',(92.0215351213467,2.05540838260006,1.61321848327588));
#26786=CARTESIAN_POINT('Ctrl Pts',(92.1406858373659,-0.242238039947421,
2.60163327433116));
#26787=CARTESIAN_POINT('Ctrl Pts',(92.2598365533851,-2.3179073918734,1.20601887651735));
#26788=CARTESIAN_POINT('Ctrl Pts',(92.3789872694042,-2.26954161474959,-1.2947420697697));
#26789=CARTESIAN_POINT('Ctrl Pts',(92.4981379854234,-0.141461063357769,
-2.6090543580659));
#26790=CARTESIAN_POINT('Ctrl Pts',(92.6172887014424,2.11624858884793,-1.53253644494961));
#26791=CARTESIAN_POINT('Ctrl Pts',(92.7364394174617,2.43471492607153,0.94833499112654));
#26792=CARTESIAN_POINT('Ctrl Pts',(92.8555901334807,0.522108464886517,2.56019115396389));
#26793=CARTESIAN_POINT('Ctrl Pts',(92.9747408494998,-1.86893675604876,1.82599326894201));
#26794=CARTESIAN_POINT('Ctrl Pts',(93.093891565519,-2.54736506743762,-0.581469883647004));
#26795=CARTESIAN_POINT('Ctrl Pts',(93.2130422815382,-0.891492618084537,
-2.45609790537574));
#26796=CARTESIAN_POINT('Ctrl Pts',(93.3321929975572,1.58130706424433,-2.08005864829791));
#26797=CARTESIAN_POINT('Ctrl Pts',(93.4513437135765,2.60506187682501,0.20206095369112));
#26798=CARTESIAN_POINT('Ctrl Pts',(93.5704944295954,1.24164494167299,2.29902019337778));
#26799=CARTESIAN_POINT('Ctrl Pts',(93.6896451456148,-1.25956443969529,2.2892517190914));
#26800=CARTESIAN_POINT('Ctrl Pts',(93.8087958616338,-2.60656068257214,0.181706959322336));
#26801=CARTESIAN_POINT('Ctrl Pts',(93.9279465776529,-1.5650117337003,-2.09234659756582));
#26802=CARTESIAN_POINT('Ctrl Pts',(94.0470972936722,0.910649713123118,-2.44905963810584));
#26803=CARTESIAN_POINT('Ctrl Pts',(94.1662480096911,2.55182915145811,-0.561554977506499));
#26804=CARTESIAN_POINT('Ctrl Pts',(94.2853987257105,1.85461712604488,1.8405356086673));
#26805=CARTESIAN_POINT('Ctrl Pts',(94.4045494417295,-0.542089888515468,
2.5560349300755));
#26806=CARTESIAN_POINT('Ctrl Pts',(94.5237001577486,-2.44204798586726,0.929288784886628));
#26807=CARTESIAN_POINT('Ctrl Pts',(94.6428508737678,-2.10421357232497,-1.54901944888943));
#26808=CARTESIAN_POINT('Ctrl Pts',(94.7620015897869,0.161835766035032,-2.60786985791601));
#26809=CARTESIAN_POINT('Ctrl Pts',(94.881152305806,2.27958545290423,-1.27697540066444));
#26810=CARTESIAN_POINT('Ctrl Pts',(95.0003030218252,2.30841662384981,1.22408688487725));
#26811=CARTESIAN_POINT('Ctrl Pts',(95.1194537378444,0.221909577540923,2.60344620654823));
#26812=CARTESIAN_POINT('Ctrl Pts',(95.2386044538635,-2.06794629466763,1.59711431443246));
#26813=CARTESIAN_POINT('Ctrl Pts',(95.3577551698827,-2.46282108627517,-0.872747562582139));
#26814=CARTESIAN_POINT('Ctrl Pts',(95.4769058859017,-0.6008677506577,-2.54285940571127));
#26815=CARTESIAN_POINT('Ctrl Pts',(95.596056601921,1.81169612178837,-1.88279929182366));
#26816=CARTESIAN_POINT('Ctrl Pts',(95.71520731794,2.56409605117663,0.502580790853675));
#26817=CARTESIAN_POINT('Ctrl Pts',(95.8343580339592,0.966863633558315,2.42741647129147));
#26818=CARTESIAN_POINT('Ctrl Pts',(95.9535087499783,-1.51636292125719,2.12786736006524));
#26819=CARTESIAN_POINT('Ctrl Pts',(96.0726594659974,-2.61005675246339,-0.121572035908453));
#26820=CARTESIAN_POINT('Ctrl Pts',(96.1918101820166,-1.31200173701596,-2.25960780956831));
#26821=CARTESIAN_POINT('Ctrl Pts',(96.3109608980357,1.18831780327526,-2.32703175943377));
#26822=CARTESIAN_POINT('Ctrl Pts',(96.4301116140548,2.59971169750167,-0.262059346079031));
#26823=CARTESIAN_POINT('Ctrl Pts',(96.549262330074,1.62883652870388,2.04305349263221));
#26824=CARTESIAN_POINT('Ctrl Pts',(96.6684130460932,-0.834637559730204,
2.47599599250058));
#26825=CARTESIAN_POINT('Ctrl Pts',(96.7875637621122,-2.5332840562059,0.640037422004922));
#26826=CARTESIAN_POINT('Ctrl Pts',(96.9067144781315,-1.91053305281782,-1.78242516395526));
#26827=CARTESIAN_POINT('Ctrl Pts',(97.0258651941505,0.462951999272051,-2.57154651082474));
#26828=CARTESIAN_POINT('Ctrl Pts',(97.1450159101697,2.41220684667701,-1.00420821538247));
#26829=CARTESIAN_POINT('Ctrl Pts',(97.2641666261889,2.15101437796858,1.48334525882557));
#26830=CARTESIAN_POINT('Ctrl Pts',(97.383317342208,-0.0812793523782635,
2.61162203957959));
#26831=CARTESIAN_POINT('Ctrl Pts',(97.5024680582271,-2.23909202123227,1.34671560900866));
#26832=CARTESIAN_POINT('Ctrl Pts',(97.6216187742462,-2.34509269253657,-1.15226571380024));
#26833=CARTESIAN_POINT('Ctrl Pts',(97.7407694902653,-0.302146702791784,
-2.59535804444827));
#26834=CARTESIAN_POINT('Ctrl Pts',(97.8599202062845,2.0176741196083,-1.66017082237124));
#26835=CARTESIAN_POINT('Ctrl Pts',(97.9790709223037,2.48858121964347,0.796328782331391));
#26836=CARTESIAN_POINT('Ctrl Pts',(98.0982216383227,0.679054661798639,2.52310538032613));
#26837=CARTESIAN_POINT('Ctrl Pts',(98.217372354342,-1.75272970399117,1.93781181010375));
#26838=CARTESIAN_POINT('Ctrl Pts',(98.3365230703609,-2.57838453922373,-0.423212963874765));
#26839=CARTESIAN_POINT('Ctrl Pts',(98.4556737863803,-1.0413136272748,-2.39642271009119));
#26840=CARTESIAN_POINT('Ctrl Pts',(98.5748245023993,1.44997430680488,-2.17364916164441));
#26841=CARTESIAN_POINT('Ctrl Pts',(98.6939752184185,2.61256538278553,0.040967407633777));
#26842=CARTESIAN_POINT('Ctrl Pts',(98.8131259344376,1.38110867692141,2.2180427824181));
#26843=CARTESIAN_POINT('Ctrl Pts',(98.9322766504567,-1.11593905853341,2.3625955031882));
#26844=CARTESIAN_POINT('Ctrl Pts',(99.0514273664759,-2.59038657112374,0.342161340890021));
#26845=CARTESIAN_POINT('Ctrl Pts',(99.1705780824951,-1.69110916152168,-1.99181270690224));
#26846=CARTESIAN_POINT('Ctrl Pts',(99.289728798514,0.757829215904196,-2.50057678394453));
#26847=CARTESIAN_POINT('Ctrl Pts',(99.4088795145334,2.512328068901,-0.717904175599352));
#26848=CARTESIAN_POINT('Ctrl Pts',(99.5280302305524,1.96462455235365,1.72260485940214));
#26849=CARTESIAN_POINT('Ctrl Pts',(99.6471809465717,-0.383364156825967,
2.58463231854081));
#26850=CARTESIAN_POINT('Ctrl Pts',(99.7663316625907,-2.38008573047184,1.07812360750406));
#26851=CARTESIAN_POINT('Ctrl Pts',(99.8854823786097,-2.19573064837981,-1.41616355462039));
#26852=CARTESIAN_POINT('Ctrl Pts',(100.004633094629,0.000574748323657545,
-2.6130746980439));
#26853=CARTESIAN_POINT('Ctrl Pts',(100.123783810648,2.19660668513872,-1.41479796477074));
#26854=CARTESIAN_POINT('Ctrl Pts',(100.242934526667,2.37925330024036,1.07859928057243));
#26855=CARTESIAN_POINT('Ctrl Pts',(100.362085242686,0.382666358997397,2.58629611947964));
#26856=CARTESIAN_POINT('Ctrl Pts',(100.481250807047,-1.96701948147245,1.71843727007359));
#26857=CARTESIAN_POINT('Ctrl Pts',(100.56069946607,-2.32733414825746,0.0980738212602812));
#26858=CARTESIAN_POINT('Ctrl Pts',(100.600431219751,-2.12456919163931,-0.60910026033635));
#26859=CARTESIAN_POINT('Ctrl Pts',(100.349869898682,0.479414994925324,2.1549256777474));
#26860=CARTESIAN_POINT('Ctrl Pts',(100.349869898682,0.426652918711037,2.16183856744932));
#26861=CARTESIAN_POINT('Ctrl Pts',(100.349869898682,0.373742092670596,2.16669187525473));
#26862=CARTESIAN_POINT('Ctrl Pts',(100.349869898682,0.320765011501736,2.16941984999731));
#26863=CARTESIAN_POINT('Ctrl Pts',(100.349869898682,0.243016014546236,2.17342341711117));
#26864=CARTESIAN_POINT('Ctrl Pts',(100.349869898682,0.16512364757463,2.17285169457014));
#26865=CARTESIAN_POINT('Ctrl Pts',(100.349869898682,0.0874187569404108,
2.16789484102443));
#26866=CARTESIAN_POINT('Ctrl Pts',(100.349869898682,0.00882392242687584,
2.16288121728784));
#26867=CARTESIAN_POINT('Ctrl Pts',(100.349869898682,-0.0695801139311062,
2.15338096217544));
#26868=CARTESIAN_POINT('Ctrl Pts',(100.349869898682,-0.147434733898743,
2.13954043576136));
#26869=CARTESIAN_POINT('Ctrl Pts',(100.349869898682,-0.214042289617913,
2.12769934483199));
#26870=CARTESIAN_POINT('Ctrl Pts',(100.349869898682,-0.280247772641109,
2.11268039048099));
#26871=CARTESIAN_POINT('Ctrl Pts',(100.349869898682,-0.345809014350907,
2.09455055013332));
#26872=CARTESIAN_POINT('Ctrl Pts',(100.349869898682,-0.357788807056817,
2.09123774330581));
#26873=CARTESIAN_POINT('Ctrl Pts',(100.349869898682,-0.369741677068303,
2.08782245032927));
#26874=CARTESIAN_POINT('Ctrl Pts',(100.349869898682,-0.381659087973601,
2.08430749424));
#26875=CARTESIAN_POINT('Ctrl Pts',(100.349869898682,-0.455832594990877,
2.06243054275909));
#26876=CARTESIAN_POINT('Ctrl Pts',(100.349869898682,-0.528720372073745,
2.03667310778326));
#26877=CARTESIAN_POINT('Ctrl Pts',(100.349869898682,-0.599998286829302,
2.00720683896365));
#26878=CARTESIAN_POINT('Ctrl Pts',(100.349869898682,-0.671071640285958,
1.97782513572434));
#26879=CARTESIAN_POINT('Ctrl Pts',(100.349869898682,-0.740545253992376,
1.94475525166359));
#26880=CARTESIAN_POINT('Ctrl Pts',(100.349869898682,-0.808069062003364,
1.90812458173475));
#26881=CARTESIAN_POINT('Ctrl Pts',(100.349869898682,-0.875592870014457,
1.87149391180587));
#26882=CARTESIAN_POINT('Ctrl Pts',(100.349869898682,-0.941167756180382,
1.83130189692078));
#26883=CARTESIAN_POINT('Ctrl Pts',(100.349869898682,-1.00440156213989,1.78764176103565));
#26884=CARTESIAN_POINT('Ctrl Pts',(100.349869898682,-1.02779687561389,1.77148833566688));
#26885=CARTESIAN_POINT('Ctrl Pts',(100.349869898682,-1.05087124668116,1.75485987879234));
#26886=CARTESIAN_POINT('Ctrl Pts',(100.349869898682,-1.07360298298091,1.73776016033232));
#26887=CARTESIAN_POINT('Ctrl Pts',(100.349869898682,-1.0834417566988,1.7303590424261));
#26888=CARTESIAN_POINT('Ctrl Pts',(100.349869898682,-1.09320813055685,1.72287579541146));
#26889=CARTESIAN_POINT('Ctrl Pts',(100.349869898682,-1.10289990339264,1.71531171169829));
#26890=CARTESIAN_POINT('Ctrl Pts',(100.349869898682,-1.16103677703682,1.66993795124006));
#26891=CARTESIAN_POINT('Ctrl Pts',(100.349869898682,-1.21650251586315,1.62165059602811));
#26892=CARTESIAN_POINT('Ctrl Pts',(100.349869898682,-1.26898476694497,1.57056955339216));
#26893=CARTESIAN_POINT('Ctrl Pts',(100.349869898682,-1.31991541650645,1.52099868651621));
#26894=CARTESIAN_POINT('Ctrl Pts',(100.349869898682,-1.36803686624987,1.46879626023262));
#26895=CARTESIAN_POINT('Ctrl Pts',(100.349869898682,-1.41302321718474,1.41404528417547));
#26896=CARTESIAN_POINT('Ctrl Pts',(100.349869898682,-1.44122551234148,1.37972146917835));
#26897=CARTESIAN_POINT('Ctrl Pts',(100.349869898682,-1.46819484166188,1.34439554635872));
#26898=CARTESIAN_POINT('Ctrl Pts',(100.349869898682,-1.49384116343081,1.30808394627531));
#26899=CARTESIAN_POINT('Ctrl Pts',(100.349869898682,-1.52549362611721,1.26326849175988));
#26900=CARTESIAN_POINT('Ctrl Pts',(100.349869898682,-1.55513111765511,1.21695133144359));
#26901=CARTESIAN_POINT('Ctrl Pts',(100.349869898682,-1.58271301197475,1.16927838686888));
#26902=CARTESIAN_POINT('Ctrl Pts',(100.349869898682,-1.58818639734863,1.1598181085232));
#26903=CARTESIAN_POINT('Ctrl Pts',(100.349869898682,-1.59357707452801,1.15030730513006));
#26904=CARTESIAN_POINT('Ctrl Pts',(100.349869898682,-1.59888102457638,1.14075431016912));
#26905=CARTESIAN_POINT('Ctrl Pts',(100.349869898682,-1.63352381179593,1.07835885607847));
#26906=CARTESIAN_POINT('Ctrl Pts',(100.349869898682,-1.66452248560294,1.01407626558591));
#26907=CARTESIAN_POINT('Ctrl Pts',(100.349869898682,-1.69186815495425,0.948254794830066));
#26908=CARTESIAN_POINT('Ctrl Pts',(100.349869898682,-1.71949907167233,0.881746729024396));
#26909=CARTESIAN_POINT('Ctrl Pts',(100.349869898682,-1.74340046296127,0.813666407870188));
#26910=CARTESIAN_POINT('Ctrl Pts',(100.349869898682,-1.76351145671393,0.744362695339321));
#26911=CARTESIAN_POINT('Ctrl Pts',(100.349869898682,-1.77818378696145,0.693800949354107));
#26912=CARTESIAN_POINT('Ctrl Pts',(100.349869898682,-1.79083752897198,0.642587752401212));
#26913=CARTESIAN_POINT('Ctrl Pts',(100.349869898682,-1.80143159096359,0.590860235567238));
#26914=CARTESIAN_POINT('Ctrl Pts',(100.349869898682,-1.80788893402656,0.559331033429622));
#26915=CARTESIAN_POINT('Ctrl Pts',(100.349869898682,-1.81358077732524,0.527610800354061));
#26916=CARTESIAN_POINT('Ctrl Pts',(100.349869898682,-1.81849513035551,0.495731460558721));
#26917=CARTESIAN_POINT('Ctrl Pts',(100.349869898682,-1.82044661710907,0.483072193115095));
#26918=CARTESIAN_POINT('Ctrl Pts',(100.349869898682,-1.82227577945532,0.470385589327665));
#26919=CARTESIAN_POINT('Ctrl Pts',(100.349869898682,-1.82398080210445,0.457681045001183));
#26920=CARTESIAN_POINT('Ctrl Pts',(100.349869898682,-1.83331587288179,0.388123130012532));
#26921=CARTESIAN_POINT('Ctrl Pts',(100.349869898682,-1.83891415246051,0.31818414360954));
#26922=CARTESIAN_POINT('Ctrl Pts',(100.349869898682,-1.84071131029445,0.248192856326947));
#26923=CARTESIAN_POINT('Ctrl Pts',(100.349869898682,-1.84233496365043,0.184958795110429));
#26924=CARTESIAN_POINT('Ctrl Pts',(100.349869898682,-1.84085536620104,0.121681523396419));
#26925=CARTESIAN_POINT('Ctrl Pts',(100.349869898682,-1.83619001506015,0.0586141186189469));
#26926=CARTESIAN_POINT('Ctrl Pts',(100.349869898682,-1.83446389372265,0.0352799708132087));
#26927=CARTESIAN_POINT('Ctrl Pts',(100.349869898682,-1.83230134629309,0.0119746999217672));
#26928=CARTESIAN_POINT('Ctrl Pts',(100.349869898682,-1.82969704876538,-0.0112882622057083));
#26929=CARTESIAN_POINT('Ctrl Pts',(100.349869898682,-1.82803245302927,-0.0261573112120664));
#26930=CARTESIAN_POINT('Ctrl Pts',(100.349869898682,-1.82618711014666,-0.0410101441524499));
#26931=CARTESIAN_POINT('Ctrl Pts',(100.349869898682,-1.82416216292868,-0.0558261756737488));
#26932=CARTESIAN_POINT('Ctrl Pts',(100.349869898682,-1.81512268037586,-0.121965805017932));
#26933=CARTESIAN_POINT('Ctrl Pts',(100.349869898682,-1.80249961741194,-0.187453075270775));
#26934=CARTESIAN_POINT('Ctrl Pts',(100.349869898682,-1.78620616216057,-0.251987814725561));
#26935=CARTESIAN_POINT('Ctrl Pts',(100.349869898682,-1.77003269803693,-0.316047296106174));
#26936=CARTESIAN_POINT('Ctrl Pts',(100.349869898682,-1.75024259013835,-0.379169001456227));
#26937=CARTESIAN_POINT('Ctrl Pts',(100.349869898682,-1.72670765863925,-0.441032704914));
#26938=CARTESIAN_POINT('Ctrl Pts',(100.349869898682,-1.72060689789578,-0.457069108228596));
#26939=CARTESIAN_POINT('Ctrl Pts',(100.349869898682,-1.71425427817134,-0.473020805173369));
#26940=CARTESIAN_POINT('Ctrl Pts',(100.349869898682,-1.70764710160355,-0.488881825071062));
#26941=CARTESIAN_POINT('',(90.3490368852675,0.43141198410659,1.72456317283204));
#26942=CARTESIAN_POINT('Ctrl Pts',(90.3498698986825,0.431841315399937,1.72595542684201));
#26943=CARTESIAN_POINT('Ctrl Pts',(90.3498698986825,0.474841144465499,1.72062771663675));
#26944=CARTESIAN_POINT('Ctrl Pts',(90.3498698986825,0.517549233669024,1.71363307981672));
#26945=CARTESIAN_POINT('Ctrl Pts',(90.3498698986825,0.55987274194016,1.70495472032253));
#26946=CARTESIAN_POINT('Ctrl Pts',(90.3498698986825,0.624504400691931,1.69170211456593));
#26947=CARTESIAN_POINT('Ctrl Pts',(90.3498698986825,0.688239505721175,1.67452610531965));
#26948=CARTESIAN_POINT('Ctrl Pts',(90.3498698986825,0.750879107318416,1.65371126258147));
#26949=CARTESIAN_POINT('Ctrl Pts',(90.3498698986825,0.78576267441883,1.64211961856032));
#26950=CARTESIAN_POINT('Ctrl Pts',(90.3498698986825,0.82030656319226,1.62939848267545));
#26951=CARTESIAN_POINT('Ctrl Pts',(90.3498698986825,0.854476163578898,1.61559006912157));
#26952=CARTESIAN_POINT('Ctrl Pts',(90.3498698986825,0.86779419338757,1.61020806695472));
#26953=CARTESIAN_POINT('Ctrl Pts',(90.3498698986825,0.881057426269843,1.6046599411249));
#26954=CARTESIAN_POINT('Ctrl Pts',(90.3498698986825,0.894257109673284,1.59895090028478));
#26955=CARTESIAN_POINT('Ctrl Pts',(90.3498698986825,0.95740243452862,1.57163969686851));
#26956=CARTESIAN_POINT('Ctrl Pts',(90.3498698986825,1.01896094569028,1.54070914056002));
#26957=CARTESIAN_POINT('Ctrl Pts',(90.3498698986825,1.07871772693759,1.50646956606796));
#26958=CARTESIAN_POINT('Ctrl Pts',(90.3498698986825,1.1384745081849,1.4722299915759));
#26959=CARTESIAN_POINT('Ctrl Pts',(90.3498698986825,1.19643034452649,1.43468089597475));
#26960=CARTESIAN_POINT('Ctrl Pts',(90.3498698986825,1.25236316356459,1.39408084780543));
#26961=CARTESIAN_POINT('Ctrl Pts',(90.3498698986825,1.26444032963695,1.38531437522781));
#26962=CARTESIAN_POINT('Ctrl Pts',(90.3498698986825,1.27642312556603,1.37640548370779));
#26963=CARTESIAN_POINT('Ctrl Pts',(90.3498698986825,1.28830921630361,1.3673564950876));
#26964=CARTESIAN_POINT('Ctrl Pts',(90.3498698986825,1.30329584009538,1.35594704254841));
#26965=CARTESIAN_POINT('Ctrl Pts',(90.3498698986825,1.31813332928755,1.34431096898488));
#26966=CARTESIAN_POINT('Ctrl Pts',(90.3498698986825,1.33279071859542,1.33247444330211));
#26967=CARTESIAN_POINT('Ctrl Pts',(90.3498698986825,1.38865459604757,1.2873617560211));
#26968=CARTESIAN_POINT('Ctrl Pts',(90.3498698986825,1.44196466536913,1.23929766435431));
#26969=CARTESIAN_POINT('Ctrl Pts',(90.3498698986825,1.49249617721103,1.18859455163048));
#26970=CARTESIAN_POINT('Ctrl Pts',(90.3498698986825,1.54366615097348,1.13725080882164));
#26971=CARTESIAN_POINT('Ctrl Pts',(90.3498698986825,1.59198784076943,1.08320041802009));
#26972=CARTESIAN_POINT('Ctrl Pts',(90.3498698986825,1.63721050702468,1.02671705930785));
#26973=CARTESIAN_POINT('Ctrl Pts',(90.3498698986825,1.6821386474709,0.970601564949918));
#26974=CARTESIAN_POINT('Ctrl Pts',(90.3498698986825,1.72400888489749,0.912084010178768));
#26975=CARTESIAN_POINT('Ctrl Pts',(90.3498698986825,1.76254479103065,0.851392268311232));
#26976=CARTESIAN_POINT('Ctrl Pts',(90.3498698986825,1.77300783767251,0.834913597127501));
#26977=CARTESIAN_POINT('Ctrl Pts',(90.3498698986825,1.7832248602594,0.818274445593801));
#26978=CARTESIAN_POINT('Ctrl Pts',(90.3498698986825,1.79318980004416,0.801478956440628));
#26979=CARTESIAN_POINT('Ctrl Pts',(90.3498698986825,1.79955534257004,0.790750100797067));
#26980=CARTESIAN_POINT('Ctrl Pts',(90.3498698986825,1.80581833349577,0.779956701588126));
#26981=CARTESIAN_POINT('Ctrl Pts',(90.3498698986825,1.8119692394867,0.769114285455295));
#26982=CARTESIAN_POINT('Ctrl Pts',(90.3498698986825,1.84875184073079,0.704276313663121));
#26983=CARTESIAN_POINT('Ctrl Pts',(90.3498698986825,1.88159981518028,0.637570922779398));
#26984=CARTESIAN_POINT('Ctrl Pts',(90.3498698986825,1.91026209575643,0.56929255805336));
#26985=CARTESIAN_POINT('Ctrl Pts',(90.3498698986825,1.9192117974947,0.547972865858894));
#26986=CARTESIAN_POINT('Ctrl Pts',(90.3498698986825,1.9277531868049,0.526499495860398));
#26987=CARTESIAN_POINT('Ctrl Pts',(90.3498698986825,1.93587796203388,0.504880604295509));
#26988=CARTESIAN_POINT('Ctrl Pts',(90.3498698986825,1.96125429222847,0.437357735621539));
#26989=CARTESIAN_POINT('Ctrl Pts',(90.3498698986825,1.98257013429095,0.368417422671432));
#26990=CARTESIAN_POINT('Ctrl Pts',(90.3498698986825,1.99995022625152,0.298378990239343));
#26991=CARTESIAN_POINT('Ctrl Pts',(90.3498698986825,2.01733031821208,0.228340557807258));
#26992=CARTESIAN_POINT('Ctrl Pts',(90.3498698986825,2.03077467779787,0.157203167161218));
#26993=CARTESIAN_POINT('Ctrl Pts',(90.3498698986825,2.04036047300214,0.0852645536046799));
#26994=CARTESIAN_POINT('Ctrl Pts',(90.3498698986825,2.04251882481325,0.0690667490876816));
#26995=CARTESIAN_POINT('Ctrl Pts',(90.3498698986825,2.04448173438142,0.0528237008312667));
#26996=CARTESIAN_POINT('Ctrl Pts',(90.3498698986825,2.04624695875266,0.0365679053387177));
#26997=CARTESIAN_POINT('Ctrl Pts',(90.3498698986825,2.05428355565192,-0.0374404064539693));
#26998=CARTESIAN_POINT('Ctrl Pts',(90.3498698986825,2.05824267691534,-0.1118154870067));
#26999=CARTESIAN_POINT('Ctrl Pts',(90.3498698986825,2.0582761742277,-0.18621558070567));
#27000=CARTESIAN_POINT('Ctrl Pts',(90.3498698986825,2.05831029294659,-0.261995865834513));
#27001=CARTESIAN_POINT('Ctrl Pts',(90.3498698986825,2.05427191440651,-0.337802955295744));
#27002=CARTESIAN_POINT('Ctrl Pts',(90.3498698986825,2.04627147702015,-0.413297832844443));
#27003=CARTESIAN_POINT('Ctrl Pts',(90.3498698986825,2.03818548363352,-0.489600046223829));
#27004=CARTESIAN_POINT('Ctrl Pts',(90.3498698986825,2.02605230739823,-0.565584325798713));
#27005=CARTESIAN_POINT('Ctrl Pts',(90.3498698986825,2.00993395348048,-0.640908956132829));
#27006=CARTESIAN_POINT('Ctrl Pts',(90.3498698986825,2.0038696133045,-0.669248958114903));
#27007=CARTESIAN_POINT('Ctrl Pts',(90.3498698986825,1.997240622828,-0.697495588968377));
#27008=CARTESIAN_POINT('Ctrl Pts',(90.3498698986825,1.99004837701445,-0.725630494083074));
#27009=CARTESIAN_POINT('Ctrl Pts',(90.3498698986825,1.9868300478939,-0.738220078307771));
#27010=CARTESIAN_POINT('Ctrl Pts',(90.3498698986825,1.98349864718324,-0.750787978975288));
#27011=CARTESIAN_POINT('Ctrl Pts',(90.3498698986825,1.98005882552642,-0.763316755998213));
#27012=CARTESIAN_POINT('Ctrl Pts',(90.3498698986825,1.9590923373259,-0.839682475452813));
#27013=CARTESIAN_POINT('Ctrl Pts',(90.3498698986825,1.93406748684485,-0.914733173083993));
#27014=CARTESIAN_POINT('Ctrl Pts',(90.3498698986825,1.9051109069263,-0.988108398973491));
#27015=CARTESIAN_POINT('Ctrl Pts',(90.3498698986825,1.87610067910297,-1.06161956726859));
#27016=CARTESIAN_POINT('Ctrl Pts',(90.3498698986825,1.84314408918446,-1.13345011149863));
#27017=CARTESIAN_POINT('Ctrl Pts',(90.3498698986825,1.80631634284738,-1.20323986435587));
#27018=CARTESIAN_POINT('Ctrl Pts',(90.3498698986825,1.77027623607485,-1.27153701513948));
#27019=CARTESIAN_POINT('Ctrl Pts',(90.3498698986825,1.73052856007933,-1.33788070101697));
#27020=CARTESIAN_POINT('Ctrl Pts',(90.3498698986825,1.68709628884852,-1.40192061396576));
#27021=CARTESIAN_POINT('Ctrl Pts',(90.3498698986825,1.66663353523184,-1.43209248670392));
#27022=CARTESIAN_POINT('Ctrl Pts',(90.3498698986825,1.64535222417335,-1.46175270636565));
#27023=CARTESIAN_POINT('Ctrl Pts',(90.3498698986825,1.62325119196239,-1.49086269246791));
#27024=CARTESIAN_POINT('Ctrl Pts',(90.3490368852675,0.431058928865748,1.7231518396082));
#27025=CARTESIAN_POINT('Ctrl Pts',(90.3493145564058,0.423441373996219,1.72505742620083));
#27026=CARTESIAN_POINT('Ctrl Pts',(90.3495922275442,0.415811182876356,1.72691249954867));
#27027=CARTESIAN_POINT('Ctrl Pts',(90.3498698986825,0.408169026503128,1.72871689651704));
#27028=CARTESIAN_POINT('Origin',(90.3498698986825,-2.40291074888303E-16,
0.));
#27029=CARTESIAN_POINT('Ctrl Pts',(90.3498698986825,-0.214101726762248,
-2.19357617843498));
#27030=CARTESIAN_POINT('Ctrl Pts',(90.3498698986825,-0.253065554508827,
-2.18618780244257));
#27031=CARTESIAN_POINT('Ctrl Pts',(90.3498698986825,-0.291777125231032,
-2.17767057969179));
#27032=CARTESIAN_POINT('Ctrl Pts',(90.3498698986825,-0.330194078040922,
-2.16800471972978));
#27033=CARTESIAN_POINT('Ctrl Pts',(90.3498698986825,-0.406738639557457,
-2.14874579994681));
#27034=CARTESIAN_POINT('Ctrl Pts',(90.3498698986825,-0.482115441150976,
-2.12492954084015));
#27035=CARTESIAN_POINT('Ctrl Pts',(90.3498698986825,-0.556039436089016,
-2.09682490938438));
#27036=CARTESIAN_POINT('Ctrl Pts',(90.3498698986825,-0.591892015180994,
-2.08319437544255));
#27037=CARTESIAN_POINT('Ctrl Pts',(90.3498698986825,-0.627402453821627,
-2.06855445597946));
#27038=CARTESIAN_POINT('Ctrl Pts',(90.3498698986825,-0.662535477352677,
-2.05293241695312));
#27039=CARTESIAN_POINT('Ctrl Pts',(90.3498698986825,-0.679780447079462,
-2.04526437238981));
#27040=CARTESIAN_POINT('Ctrl Pts',(90.3498698986825,-0.696934454724013,
-2.03735967383536));
#27041=CARTESIAN_POINT('Ctrl Pts',(90.3498698986825,-0.713993138554709,
-2.02922138301725));
#27042=CARTESIAN_POINT('Ctrl Pts',(90.3498698986825,-0.726153529799601,
-2.02341995065617));
#27043=CARTESIAN_POINT('Ctrl Pts',(90.3498698986825,-0.738263467090769,
-2.01750071137785));
#27044=CARTESIAN_POINT('Ctrl Pts',(90.3498698986825,-0.750313634121252,
-2.01146892060575));
#27045=CARTESIAN_POINT('Ctrl Pts',(90.3498698986825,-0.820320629230508,
-1.97642645637979));
#27046=CARTESIAN_POINT('Ctrl Pts',(90.3498698986825,-0.888389925908362,
-1.93755209172309));
#27047=CARTESIAN_POINT('Ctrl Pts',(90.3498698986825,-0.954242008517751,
-1.89510921264174));
#27048=CARTESIAN_POINT('Ctrl Pts',(90.3498698986825,-1.00375379708154,-1.86319795377422));
#27049=CARTESIAN_POINT('Ctrl Pts',(90.3498698986825,-1.0520116823982,-1.82926838600638));
#27050=CARTESIAN_POINT('Ctrl Pts',(90.3498698986825,-1.09888241457236,-1.7934195088416));
#27051=CARTESIAN_POINT('Ctrl Pts',(90.3498698986825,-1.12145931356829,-1.77615166510791));
#27052=CARTESIAN_POINT('Ctrl Pts',(90.3498698986825,-1.14371416086655,-1.75843836186297));
#27053=CARTESIAN_POINT('Ctrl Pts',(90.3498698986825,-1.16563083104683,-1.74028997732421));
#27054=CARTESIAN_POINT('Ctrl Pts',(90.3498698986825,-1.17633935367306,-1.73142264552316));
#27055=CARTESIAN_POINT('Ctrl Pts',(90.3498698986825,-1.18696862372856,-1.72245015180798));
#27056=CARTESIAN_POINT('Ctrl Pts',(90.3498698986825,-1.19751194217376,-1.7133777644169));
#27057=CARTESIAN_POINT('Ctrl Pts',(90.3498698986825,-1.25555020266794,-1.66343660163746));
#27058=CARTESIAN_POINT('Ctrl Pts',(90.3498698986825,-1.31081695977831,-1.61061924094653));
#27059=CARTESIAN_POINT('Ctrl Pts',(90.3498698986825,-1.36305428431188,-1.55517048742002));
#27060=CARTESIAN_POINT('Ctrl Pts',(90.3498698986825,-1.41423592353542,-1.50084232027651));
#27061=CARTESIAN_POINT('Ctrl Pts',(90.3498698986825,-1.46250982428705,-1.44398719088105));
#27062=CARTESIAN_POINT('Ctrl Pts',(90.3498698986825,-1.50759196665253,-1.38480940421943));
#27063=CARTESIAN_POINT('Ctrl Pts',(90.3498698986825,-1.55169882702195,-1.32691183688347));
#27064=CARTESIAN_POINT('Ctrl Pts',(90.3498698986825,-1.59275091350146,-1.26679030650822));
#27065=CARTESIAN_POINT('Ctrl Pts',(90.3498698986825,-1.63043591394234,-1.20462243846732));
#27066=CARTESIAN_POINT('Ctrl Pts',(90.3498698986825,-1.64313694391479,-1.18366991236746));
#27067=CARTESIAN_POINT('Ctrl Pts',(90.3498698986825,-1.6554550854017,-1.16248487188985));
#27068=CARTESIAN_POINT('Ctrl Pts',(90.3498698986825,-1.66737704460729,-1.14107396752519));
#27069=CARTESIAN_POINT('Ctrl Pts',(90.3498698986825,-1.67411655420061,-1.12897033649619));
#27070=CARTESIAN_POINT('Ctrl Pts',(90.3498698986825,-1.68072944440791,-1.11679452622329));
#27071=CARTESIAN_POINT('Ctrl Pts',(90.3498698986825,-1.68721321125449,-1.10454773595022));
#27072=CARTESIAN_POINT('Ctrl Pts',(90.3498698986825,-1.69280679091002,-1.09398236576683));
#27073=CARTESIAN_POINT('Ctrl Pts',(90.3498698986825,-1.69830255810943,-1.08336726810866));
#27074=CARTESIAN_POINT('Ctrl Pts',(90.3498698986825,-1.7036947776161,-1.07271211575908));
#27075=CARTESIAN_POINT('Ctrl Pts',(90.3498698986825,-1.73609336482417,-1.00869174674665));
#27076=CARTESIAN_POINT('Ctrl Pts',(90.3498698986825,-1.76480709245594,-0.9431339500233));
#27077=CARTESIAN_POINT('Ctrl Pts',(90.3498698986825,-1.78957581068588,-0.876226598183046));
#27078=CARTESIAN_POINT('Ctrl Pts',(90.3498698986825,-1.79745850836397,-0.854933190017841));
#27079=CARTESIAN_POINT('Ctrl Pts',(90.3498698986825,-1.80494126152076,-0.833502987124966));
#27080=CARTESIAN_POINT('Ctrl Pts',(90.3498698986825,-1.81201458800382,-0.811941804694486));
#27081=CARTESIAN_POINT('Ctrl Pts',(90.3498698986825,-1.8348025884842,-0.74247855614232));
#27082=CARTESIAN_POINT('Ctrl Pts',(90.3498698986825,-1.85334501760212,-0.671655559779614));
#27083=CARTESIAN_POINT('Ctrl Pts',(90.3498698986825,-1.86769676549779,-0.599832699437972));
#27084=CARTESIAN_POINT('Ctrl Pts',(90.3498698986825,-1.88119220525484,-0.532295205610333));
#27085=CARTESIAN_POINT('Ctrl Pts',(90.3498698986825,-1.89098144653552,-0.463872822086227));
#27086=CARTESIAN_POINT('Ctrl Pts',(90.3498698986825,-1.8970692592514,-0.394874641297999));
#27087=CARTESIAN_POINT('Ctrl Pts',(90.3498698986825,-1.89846100872212,-0.379100801649089));
#27088=CARTESIAN_POINT('Ctrl Pts',(90.3498698986825,-1.89965930467989,-0.363292543085896));
#27089=CARTESIAN_POINT('Ctrl Pts',(90.3498698986825,-1.90066249818027,-0.347482308863442));
#27090=CARTESIAN_POINT('Ctrl Pts',(90.3498698986825,-1.90518355320309,-0.27623091138485));
#27091=CARTESIAN_POINT('Ctrl Pts',(90.3498698986825,-1.90575774275523,-0.204834546543544));
#27092=CARTESIAN_POINT('Ctrl Pts',(90.3498698986825,-1.90246416416827,-0.133627830062588));
#27093=CARTESIAN_POINT('Ctrl Pts',(90.3498698986825,-1.89918981650835,-0.0628368835816743));
#27094=CARTESIAN_POINT('Ctrl Pts',(90.3498698986825,-1.8920923557442,0.00776763413713237));
#27095=CARTESIAN_POINT('Ctrl Pts',(90.3498698986825,-1.88120052057599,0.0778439105212068));
#27096=CARTESIAN_POINT('Ctrl Pts',(90.3498698986825,-1.87040101393505,0.14732616034363));
#27097=CARTESIAN_POINT('Ctrl Pts',(90.3498698986825,-1.85587082135331,0.21629000314705));
#27098=CARTESIAN_POINT('Ctrl Pts',(90.3498698986825,-1.8375952377848,0.284375112098305));
#27099=CARTESIAN_POINT('Ctrl Pts',(90.3498698986825,-1.83323021278472,0.300636874771505));
#27100=CARTESIAN_POINT('Ctrl Pts',(90.3498698986825,-1.82865134630035,0.316848351257566));
#27101=CARTESIAN_POINT('Ctrl Pts',(90.3498698986825,-1.82385810846294,0.333004312157772));
#27102=CARTESIAN_POINT('Ctrl Pts',(90.3498698986825,-1.81904913961758,0.34921329557804));
#27103=CARTESIAN_POINT('Ctrl Pts',(90.3498698986825,-1.81402317448659,0.365369472788698));
#27104=CARTESIAN_POINT('Ctrl Pts',(90.3498698986825,-1.8087903340904,0.381436299405338));
#27105=CARTESIAN_POINT('Ctrl Pts',(90.3498698986825,-1.78750081560853,0.446803284885943));
#27106=CARTESIAN_POINT('Ctrl Pts',(90.3498698986825,-1.76275858577996,0.510807133920073));
#27107=CARTESIAN_POINT('Ctrl Pts',(90.3498698986825,-1.73459751006973,0.573134766921553));
#27108=CARTESIAN_POINT('Ctrl Pts',(90.3498698986825,-1.70726855933418,0.633620695416873));
#27109=CARTESIAN_POINT('Ctrl Pts',(90.3498698986825,-1.67671932469926,0.69252867029316));
#27110=CARTESIAN_POINT('Ctrl Pts',(90.3498698986825,-1.64294315627481,0.749542922188809));
#27111=CARTESIAN_POINT('Ctrl Pts',(90.3498698986825,-1.61044975030382,0.80439186804012));
#27112=CARTESIAN_POINT('Ctrl Pts',(90.3498698986825,-1.57496942494184,0.857488626202311));
#27113=CARTESIAN_POINT('Ctrl Pts',(90.3498698986825,-1.53646769662716,0.908516538747599));
#27114=CARTESIAN_POINT('Ctrl Pts',(90.3498698986825,-1.52109669050735,0.92888836075008));
#27115=CARTESIAN_POINT('Ctrl Pts',(90.3498698986825,-1.50524382897346,0.948930000897399));
#27116=CARTESIAN_POINT('Ctrl Pts',(90.3498698986825,-1.4889058019033,0.968619417293814));
#27117=CARTESIAN_POINT('Ctrl Pts',(90.0997129159169,-1.85158348337331,1.20554584720227));
#27118=CARTESIAN_POINT('Ctrl Pts',(90.1394446688446,-2.25287748833822,0.589243178206973));
#27119=CARTESIAN_POINT('Ctrl Pts',(90.2188933271119,-2.38405002538366,-1.06497837133754));
#27120=CARTESIAN_POINT('Ctrl Pts',(90.3380588907191,-0.393267651591904,
-2.58386764348672));
#27121=CARTESIAN_POINT('Ctrl Pts',(90.4572096067382,1.95719317887114,-1.72895644355711));
#27122=CARTESIAN_POINT('Ctrl Pts',(90.5763603227573,2.51434751199701,0.707435449009888));
#27123=CARTESIAN_POINT('Ctrl Pts',(90.6955110387765,0.767367608217681,2.49699416595646));
#27124=CARTESIAN_POINT('Ctrl Pts',(90.8146617547956,-1.68275183884718,1.99769159455853));
#27125=CARTESIAN_POINT('Ctrl Pts',(90.9338124708148,-2.59088897700703,-0.331852868955999));
#27126=CARTESIAN_POINT('Ctrl Pts',(91.052963186834,-1.12483059132128,-2.35748208545346));
#27127=CARTESIAN_POINT('Ctrl Pts',(91.1721139028529,1.37197072238487,-2.22272057647922));
#27128=CARTESIAN_POINT('Ctrl Pts',(91.2912646188722,2.61155722900937,-0.0511948499463282));
#27129=CARTESIAN_POINT('Ctrl Pts',(91.4104153348913,1.45801849094823,2.16726666247893));
#27130=CARTESIAN_POINT('Ctrl Pts',(91.5295660509104,-1.03158781574602,2.39972247460381));
#27131=CARTESIAN_POINT('Ctrl Pts',(91.6487167669297,-2.57588976083882,0.433176917311585));
#27132=CARTESIAN_POINT('Ctrl Pts',(91.7678674829486,-1.75975190745909,-1.93031708468522));
#27133=CARTESIAN_POINT('Ctrl Pts',(91.887018198968,0.668950253188048,-2.52494630594999));
#27134=CARTESIAN_POINT('Ctrl Pts',(92.0061689149869,2.48465391237723,-0.805819131213874));
#27135=CARTESIAN_POINT('Ctrl Pts',(92.1253196310062,2.02352271608646,1.651727978272));
#27136=CARTESIAN_POINT('Ctrl Pts',(92.2444703470252,-0.291881605843824,
2.59569919906983));
#27137=CARTESIAN_POINT('Ctrl Pts',(92.3636210630443,-2.33981761373509,1.16107833831933));
#27138=CARTESIAN_POINT('Ctrl Pts',(92.4827717790636,-2.24364082358645,-1.33750708770756));
#27139=CARTESIAN_POINT('Ctrl Pts',(92.6019224950827,-0.091483701489442,
-2.61045590933086));
#27140=CARTESIAN_POINT('Ctrl Pts',(92.7210732111018,2.14450532932704,-1.49129012506569));
#27141=CARTESIAN_POINT('Ctrl Pts',(92.840223927121,2.41535772310533,0.994432707684751));
#27142=CARTESIAN_POINT('Ctrl Pts',(92.9593746431402,0.47287546714399,2.56889823265659));
#27143=CARTESIAN_POINT('Ctrl Pts',(93.0785253591591,-1.90293045211532,1.78933089016224));
#27144=CARTESIAN_POINT('Ctrl Pts',(93.1976760751785,-2.53496903377393,-0.629905816124492));
#27145=CARTESIAN_POINT('Ctrl Pts',(93.3168267911975,-0.844066071326822,
-2.47192269423254));
#27146=CARTESIAN_POINT('Ctrl Pts',(93.4359775072166,1.62030438400931,-2.04877110545688));
#27147=CARTESIAN_POINT('Ctrl Pts',(93.5551282232358,2.59989442679698,0.25179020789872));
#27148=CARTESIAN_POINT('Ctrl Pts',(93.674278939255,1.19704796093923,2.32162131245874));
#27149=CARTESIAN_POINT('Ctrl Pts',(93.793429655274,-1.30272410903316,2.26401396529279));
#27150=CARTESIAN_POINT('Ctrl Pts',(93.9125803712933,-2.60873329153225,0.131757174118624));
#27151=CARTESIAN_POINT('Ctrl Pts',(94.0317310873123,-1.52420639263788,-2.12123648184726));
#27152=CARTESIAN_POINT('Ctrl Pts',(94.1508818033315,0.957040665009202,-2.43041611762311));
#27153=CARTESIAN_POINT('Ctrl Pts',(94.2700325193506,2.56129495053503,-0.512462208991841));
#27154=CARTESIAN_POINT('Ctrl Pts',(94.3891832353698,1.81848370267727,1.87509102775788));
#27155=CARTESIAN_POINT('Ctrl Pts',(94.5083339513889,-0.590711348686661,
2.54438783242932));
#27156=CARTESIAN_POINT('Ctrl Pts',(94.6274846674082,-2.45860277299606,0.88211209259215));
#27157=CARTESIAN_POINT('Ctrl Pts',(94.746635383427,-2.07353155917781,-1.58849495195136));
#27158=CARTESIAN_POINT('Ctrl Pts',(94.8657860994464,0.211638842323955,-2.60347044148789));
#27159=CARTESIAN_POINT('Ctrl Pts',(94.9849368154654,2.30287209799251,-1.232732509334));
#27160=CARTESIAN_POINT('Ctrl Pts',(95.1040875314846,2.28384791226018,1.26763088197871));
#27161=CARTESIAN_POINT('Ctrl Pts',(95.2232382475037,0.171999267854588,2.60638937826619));
#27162=CARTESIAN_POINT('Ctrl Pts',(95.3423889635229,-2.0974624438256,1.55675965904262));
#27163=CARTESIAN_POINT('Ctrl Pts',(95.461539679542,-2.44489568766324,-0.91942069572478));
#27164=CARTESIAN_POINT('Ctrl Pts',(95.5806903955612,-0.551926903599348,
-2.55308167365726));
#27165=CARTESIAN_POINT('Ctrl Pts',(95.6998411115801,1.84680503441703,-1.84720342792373));
#27166=CARTESIAN_POINT('Ctrl Pts',(95.8189918275996,2.55320066331205,0.551376198383756));
#27167=CARTESIAN_POINT('Ctrl Pts',(95.9381425436185,0.919948031306832,2.44469731438807));
#27168=CARTESIAN_POINT('Ctrl Pts',(96.0572932596377,-1.55630720620991,2.0977981836154));
#27169=CARTESIAN_POINT('Ctrl Pts',(96.1764439756568,-2.60642641738223,-0.171437073158325));
#27170=CARTESIAN_POINT('Ctrl Pts',(96.295594691676,-1.26812347191844,-2.2835744347958));
#27171=CARTESIAN_POINT('Ctrl Pts',(96.4147454076951,1.23223575776735,-2.30313794127868));
#27172=CARTESIAN_POINT('Ctrl Pts',(96.5338961237143,2.60342473103421,-0.212200398490957));
#27173=CARTESIAN_POINT('Ctrl Pts',(96.6530468397333,1.58894216979488,2.07318887715146));
#27174=CARTESIAN_POINT('Ctrl Pts',(96.7721975557526,-0.881581758524136,
2.45879298483808));
#27175=CARTESIAN_POINT('Ctrl Pts',(96.8913482717716,-2.54426035849811,0.591260152097927));
#27176=CARTESIAN_POINT('Ctrl Pts',(97.0104989877908,-1.87548322584963,-1.81807920865716));
#27177=CARTESIAN_POINT('Ctrl Pts',(97.1296497038099,0.51190973312449,-2.56140542752596));
#27178=CARTESIAN_POINT('Ctrl Pts',(97.2488004198291,2.43020963014491,-0.957564876617346));
#27179=CARTESIAN_POINT('Ctrl Pts',(97.3679511358482,2.12156519947923,1.52374881277565));
#27180=CARTESIAN_POINT('Ctrl Pts',(97.4871018518674,-0.131194474865119,
2.60876165008183));
#27181=CARTESIAN_POINT('Ctrl Pts',(97.6062525678865,-2.26373291861835,1.30321242084377));
#27182=CARTESIAN_POINT('Ctrl Pts',(97.7254032839056,-2.32187945857944,-1.19654716766928));
#27183=CARTESIAN_POINT('Ctrl Pts',(97.8445539999248,-0.252350991148042,
-2.59984005266964));
#27184=CARTESIAN_POINT('Ctrl Pts',(97.9637047159438,2.04842156151389,-1.62074626677239));
#27185=CARTESIAN_POINT('Ctrl Pts',(98.0828554319631,2.47210470191559,0.843532877857234));
#27186=CARTESIAN_POINT('Ctrl Pts',(98.2020061479821,0.630452581901348,2.53483308047208));
#27187=CARTESIAN_POINT('Ctrl Pts',(98.3211568640014,-1.78892038175012,1.90331641207747));
#27188=CARTESIAN_POINT('Ctrl Pts',(98.4403075800203,-2.56900019101066,-0.472321453153471));
#27189=CARTESIAN_POINT('Ctrl Pts',(98.5594582960397,-0.994953629969765,
-2.41514296955291));
#27190=CARTESIAN_POINT('Ctrl Pts',(98.6786090120587,1.49082744648633,-2.14482734690619));
#27191=CARTESIAN_POINT('Ctrl Pts',(98.7977597280779,2.61047574120498,0.0909214290808899));
#27192=CARTESIAN_POINT('Ctrl Pts',(98.916910444097,1.33799068516524,2.24335068661261));
#27193=CARTESIAN_POINT('Ctrl Pts',(99.0360611601162,-1.16057298546944,2.34007116379782));
#27194=CARTESIAN_POINT('Ctrl Pts',(99.1552118761353,-2.59563744310819,0.292435184249233));
#27195=CARTESIAN_POINT('Ctrl Pts',(99.2743625921544,-1.65216189369095,-2.02315385011149));
#27196=CARTESIAN_POINT('Ctrl Pts',(99.3935133081736,0.805278172691334,-2.48485265297424));
#27197=CARTESIAN_POINT('Ctrl Pts',(99.5126640241926,2.52481192829851,-0.669445101955683));
#27198=CARTESIAN_POINT('Ctrl Pts',(99.6318147402118,1.93067675396188,1.75923640532605));
#27199=CARTESIAN_POINT('Ctrl Pts',(99.750965456231,-0.432581741288383,2.57618049601852));
#27200=CARTESIAN_POINT('Ctrl Pts',(99.8701161722501,-2.39957872863425,1.03171229065444));
#27201=CARTESIAN_POINT('Ctrl Pts',(99.9892668882692,-2.1674235249011,-1.45676723838871));
#27202=CARTESIAN_POINT('Ctrl Pts',(100.108417604288,0.050309877383694,-2.61313994288172));
#27203=CARTESIAN_POINT('Ctrl Pts',(100.227593394073,2.22361276397469,-1.36892539155596));
#27204=CARTESIAN_POINT('Ctrl Pts',(100.307052278519,2.31079582958269,0.288508099625264));
#27205=CARTESIAN_POINT('Ctrl Pts',(100.346794257624,1.99370331232002,0.952286295127252));
#27206=CARTESIAN_POINT('Ctrl Pts',(90.1837056635606,-1.72966766143192,1.12616778287543));
#27207=CARTESIAN_POINT('Ctrl Pts',(90.2234374164883,-2.10453882946033,0.550444999761564));
#27208=CARTESIAN_POINT('Ctrl Pts',(90.3028860747557,-2.22707443070803,-0.994855843967151));
#27209=CARTESIAN_POINT('Ctrl Pts',(90.4220516383629,-0.367373302556414,
-2.41373524039919));
#27210=CARTESIAN_POINT('Ctrl Pts',(90.5412023543819,1.82832358306688,-1.61511488695975));
#27211=CARTESIAN_POINT('Ctrl Pts',(90.660353070401,2.34879259841948,0.660855008532327));
#27212=CARTESIAN_POINT('Ctrl Pts',(90.7795037864203,0.716840989500684,2.33258186758639));
#27213=CARTESIAN_POINT('Ctrl Pts',(90.8986545024393,-1.57195258221161,1.86615541759267));
#27214=CARTESIAN_POINT('Ctrl Pts',(91.0178052184585,-2.42029426063201,-0.310002320144315));
#27215=CARTESIAN_POINT('Ctrl Pts',(91.1369559344777,-1.05076714923659,-2.20225583249695));
#27216=CARTESIAN_POINT('Ctrl Pts',(91.2561066504968,1.28163456427962,-2.07636757189643));
#27217=CARTESIAN_POINT('Ctrl Pts',(91.375257366516,2.43960163047397,-0.0478239718485028));
#27218=CARTESIAN_POINT('Ctrl Pts',(91.4944080825351,1.36201659617765,2.02456497017342));
#27219=CARTESIAN_POINT('Ctrl Pts',(91.6135587985541,-0.963663858986451,
2.24171494183538));
#27220=CARTESIAN_POINT('Ctrl Pts',(91.7327095145733,-2.4062826541417,0.404654779155604));
#27221=CARTESIAN_POINT('Ctrl Pts',(91.8518602305924,-1.64388265169106,-1.80321712073536));
#27222=CARTESIAN_POINT('Ctrl Pts',(91.9710109466116,0.624903835250292,-2.35869352447292));
#27223=CARTESIAN_POINT('Ctrl Pts',(92.0901616626308,2.32105414672393,-0.752760707113499));
#27224=CARTESIAN_POINT('Ctrl Pts',(92.2093123786497,1.89028571253566,1.54297145937729));
#27225=CARTESIAN_POINT('Ctrl Pts',(92.3284630946691,-0.27266292831427,2.42478775802007));
#27226=CARTESIAN_POINT('Ctrl Pts',(92.4476138106881,-2.1857544617719,1.08462819646738));
#27227=CARTESIAN_POINT('Ctrl Pts',(92.5667645267073,-2.09591034445596,-1.24944015612463));
#27228=CARTESIAN_POINT('Ctrl Pts',(92.6859152427263,-0.0854600407895548,
-2.438572826183));
#27229=CARTESIAN_POINT('Ctrl Pts',(92.8050659587456,2.00330233619691,-1.39309748996006));
#27230=CARTESIAN_POINT('Ctrl Pts',(92.9242166747647,2.2563207016914,0.92895519505221));
#27231=CARTESIAN_POINT('Ctrl Pts',(93.0433673907839,0.441739414262496,2.39975147674171));
#27232=CARTESIAN_POINT('Ctrl Pts',(93.162518106803,-1.77763373595305,1.67151403331608));
#27233=CARTESIAN_POINT('Ctrl Pts',(93.281668822822,-2.36805631494502,-0.5884302434549));
#27234=CARTESIAN_POINT('Ctrl Pts',(93.4008195388413,-0.78848931241601,-2.30916120400046));
#27235=CARTESIAN_POINT('Ctrl Pts',(93.5199702548604,1.5136169229547,-1.91387164478739));
#27236=CARTESIAN_POINT('Ctrl Pts',(93.6391209708795,2.42870675481237,0.235211311819554));
#27237=CARTESIAN_POINT('Ctrl Pts',(93.7582716868987,1.11822943216551,2.16875627931995));
#27238=CARTESIAN_POINT('Ctrl Pts',(93.8774224029177,-1.21694743088614,2.11494203526961));
#27239=CARTESIAN_POINT('Ctrl Pts',(93.996573118937,-2.43696363257869,0.123081743427209));
#27240=CARTESIAN_POINT('Ctrl Pts',(94.1157238349562,-1.4238464159825,-1.98156560470953));
#27241=CARTESIAN_POINT('Ctrl Pts',(94.2348745509751,0.894025197246792,-2.27038758998694));
#27242=CARTESIAN_POINT('Ctrl Pts',(94.3540252669942,2.39264882578134,-0.47871960327938));
#27243=CARTESIAN_POINT('Ctrl Pts',(94.4731759830136,1.69874730553947,1.75162737304458));
#27244=CARTESIAN_POINT('Ctrl Pts',(94.5923266990326,-0.551816499898084,
2.3768549414126));
#27245=CARTESIAN_POINT('Ctrl Pts',(94.7114774150519,-2.29671832080214,0.82403022818876));
#27246=CARTESIAN_POINT('Ctrl Pts',(94.8306281310708,-1.93700176906645,-1.48390195387379));
#27247=CARTESIAN_POINT('Ctrl Pts',(94.9497788470901,0.197703676208935,-2.43204731008477));
#27248=CARTESIAN_POINT('Ctrl Pts',(95.0689295631092,2.15124158974171,-1.15156436409024));
#27249=CARTESIAN_POINT('Ctrl Pts',(95.1880802791283,2.13347003412901,1.18416488528859));
#27250=CARTESIAN_POINT('Ctrl Pts',(95.3072309951474,0.160674133286185,2.4347740521391));
#27251=CARTESIAN_POINT('Ctrl Pts',(95.4263817111665,-1.95935694648968,1.45425624231758));
#27252=CARTESIAN_POINT('Ctrl Pts',(95.5455324271858,-2.28391376597346,-0.858882280451714));
#27253=CARTESIAN_POINT('Ctrl Pts',(95.6646831432049,-0.515585781144895,
-2.38497634461189));
#27254=CARTESIAN_POINT('Ctrl Pts',(95.7838338592239,1.72520384507921,-1.72557600672961));
#27255=CARTESIAN_POINT('Ctrl Pts',(95.9029845752431,2.38508749950162,0.515071336610853));
#27256=CARTESIAN_POINT('Ctrl Pts',(96.0221352912623,0.859374894104378,2.28372845440529));
#27257=CARTESIAN_POINT('Ctrl Pts',(96.1412860072814,-1.45383358082807,1.95967057979992));
#27258=CARTESIAN_POINT('Ctrl Pts',(96.2604367233005,-2.43480865244838,-0.160148955785822));
#27259=CARTESIAN_POINT('Ctrl Pts',(96.3795874393196,-1.18462504109399,-2.13321456353832));
#27260=CARTESIAN_POINT('Ctrl Pts',(96.4987381553389,1.15110032067646,-2.15148992881971));
#27261=CARTESIAN_POINT('Ctrl Pts',(96.6178888713579,2.43200460939413,-0.198228257223413));
#27262=CARTESIAN_POINT('Ctrl Pts',(96.7370395873772,1.48431972506719,1.9366816506249));
#27263=CARTESIAN_POINT('Ctrl Pts',(96.8561903033962,-0.823534813482703,
2.29689600831927));
#27264=CARTESIAN_POINT('Ctrl Pts',(96.9753410194154,-2.37673586088587,0.552329167850369));
#27265=CARTESIAN_POINT('Ctrl Pts',(97.0944917354345,-1.75199374721148,-1.6983694450584));
#27266=CARTESIAN_POINT('Ctrl Pts',(97.2136424514538,0.478203504680524,-2.39275202851578));
#27267=CARTESIAN_POINT('Ctrl Pts',(97.3327931674727,2.270194698488,-0.89451489262075));
#27268=CARTESIAN_POINT('Ctrl Pts',(97.4519438834919,1.98187267822947,1.42341896504805));
#27269=CARTESIAN_POINT('Ctrl Pts',(97.5710945995111,-0.122556094591716,
2.43699012388549));
#27270=CARTESIAN_POINT('Ctrl Pts',(97.6902453155302,-2.11467949385656,1.21740359025193));
#27271=CARTESIAN_POINT('Ctrl Pts',(97.8093960315494,-2.1689974280453,-1.11776161317067));
#27272=CARTESIAN_POINT('Ctrl Pts',(97.9285467475685,-0.235735170808409,
-2.42865596089974));
#27273=CARTESIAN_POINT('Ctrl Pts',(98.0476974635877,1.91354511624583,-1.51402971035114));
#27274=CARTESIAN_POINT('Ctrl Pts',(98.1668481796068,2.30933122755397,0.787991226583058));
#27275=CARTESIAN_POINT('Ctrl Pts',(98.285998895626,0.588941007938949,2.36792931336405));
#27276=CARTESIAN_POINT('Ctrl Pts',(98.4051496116451,-1.67113055445514,1.77799428273429));
#27277=CARTESIAN_POINT('Ctrl Pts',(98.5243003276642,-2.39984672174115,-0.44122187881679));
#27278=CARTESIAN_POINT('Ctrl Pts',(98.6434510436833,-0.929441817685516,
-2.25612008839036));
#27279=CARTESIAN_POINT('Ctrl Pts',(98.7626017597025,1.39266527602884,-2.00360315082291));
#27280=CARTESIAN_POINT('Ctrl Pts',(98.8817524757218,2.43859135224549,0.0849347906938011));
#27281=CARTESIAN_POINT('Ctrl Pts',(99.0009031917407,1.24989191154976,2.09563931128596));
#27282=CARTESIAN_POINT('Ctrl Pts',(99.12005390776,-1.08415611811398,2.18599131706251));
#27283=CARTESIAN_POINT('Ctrl Pts',(99.2392046237789,-2.42473006832328,0.27318005685557));
#27284=CARTESIAN_POINT('Ctrl Pts',(99.3583553397983,-1.5433768040321,-1.88994113420365));
#27285=CARTESIAN_POINT('Ctrl Pts',(99.4775060558172,0.752255367510413,-2.32123980142798));
#27286=CARTESIAN_POINT('Ctrl Pts',(99.5966567718365,2.35856799479508,-0.625366101153133));
#27287=CARTESIAN_POINT('Ctrl Pts',(99.7158074878556,1.80355310791724,1.64340109232476));
#27288=CARTESIAN_POINT('Ctrl Pts',(99.8349582038747,-0.404098791953626,
2.40655424612925));
#27289=CARTESIAN_POINT('Ctrl Pts',(99.9541089198937,-2.24158066068779,0.963780137958278));
#27290=CARTESIAN_POINT('Ctrl Pts',(100.073259635913,-2.02471150413276,-1.36084773119917));
#27291=CARTESIAN_POINT('Ctrl Pts',(100.192410351932,0.0469972694953342,
-2.44108013199815));
#27292=CARTESIAN_POINT('Ctrl Pts',(100.311586141717,2.07720101412182,-1.2787897504754));
#27293=CARTESIAN_POINT('Ctrl Pts',(100.391045026163,2.15864359046838,0.269511547528967));
#27294=CARTESIAN_POINT('Ctrl Pts',(100.430787005268,1.86242974015249,0.889583874503776));
#27295=CARTESIAN_POINT('Ctrl Pts',(90.2676984112045,-1.60775183949052,1.04678971854859));
#27296=CARTESIAN_POINT('Ctrl Pts',(90.3074301641321,-1.95620017058246,0.511646821316155));
#27297=CARTESIAN_POINT('Ctrl Pts',(90.3868788223997,-2.07009883603241,-0.924733316596755));
#27298=CARTESIAN_POINT('Ctrl Pts',(90.5060443860065,-0.341478953520925,
-2.24360283731166));
#27299=CARTESIAN_POINT('Ctrl Pts',(90.6251951020259,1.69945398726261,-1.50127333036239));
#27300=CARTESIAN_POINT('Ctrl Pts',(90.7443458180448,2.18323768484195,0.614274568054768));
#27301=CARTESIAN_POINT('Ctrl Pts',(90.863496534064,0.66631437078369,2.16816956921632));
#27302=CARTESIAN_POINT('Ctrl Pts',(90.9826472500832,-1.46115332557605,1.73461924062682));
#27303=CARTESIAN_POINT('Ctrl Pts',(91.1017979661023,-2.249699544257,-0.288151771332628));
#27304=CARTESIAN_POINT('Ctrl Pts',(91.2209486821215,-0.976703707151896,
-2.04702957954045));
#27305=CARTESIAN_POINT('Ctrl Pts',(91.3400993981407,1.19129840617438,-1.93001456731364));
#27306=CARTESIAN_POINT('Ctrl Pts',(91.4592501141596,2.26764603193859,-0.044453093750678));
#27307=CARTESIAN_POINT('Ctrl Pts',(91.578400830179,1.26601470140709,1.8818632778679));
#27308=CARTESIAN_POINT('Ctrl Pts',(91.6975515461979,-0.895739902226873,
2.08370740906695));
#27309=CARTESIAN_POINT('Ctrl Pts',(91.8167022622172,-2.23667554744459,0.376132640999623));
#27310=CARTESIAN_POINT('Ctrl Pts',(91.9358529782361,-1.52801339592303,-1.67611715678549));
#27311=CARTESIAN_POINT('Ctrl Pts',(92.0550036942554,0.580857417312533,-2.19244074299585));
#27312=CARTESIAN_POINT('Ctrl Pts',(92.1741544102744,2.15745438107064,-0.699702283013127));
#27313=CARTESIAN_POINT('Ctrl Pts',(92.2933051262937,1.75704870898488,1.43421494048258));
#27314=CARTESIAN_POINT('Ctrl Pts',(92.4124558423127,-0.253444250784714,
2.25387631697032));
#27315=CARTESIAN_POINT('Ctrl Pts',(92.531606558332,-2.0316913098087,1.00817805461546));
#27316=CARTESIAN_POINT('Ctrl Pts',(92.6507572743511,-1.94817986532546,-1.16137322454171));
#27317=CARTESIAN_POINT('Ctrl Pts',(92.7699079903702,-0.0794363800896707,
-2.26668974303514));
#27318=CARTESIAN_POINT('Ctrl Pts',(92.8890587063892,1.86209934306679,-1.29490485485441));
#27319=CARTESIAN_POINT('Ctrl Pts',(93.0082094224086,2.09728368027748,0.863477682419669));
#27320=CARTESIAN_POINT('Ctrl Pts',(93.1273601384276,0.410603361381006,2.23060472082685));
#27321=CARTESIAN_POINT('Ctrl Pts',(93.2465108544467,-1.6523370197908,1.55369717646994));
#27322=CARTESIAN_POINT('Ctrl Pts',(93.3656615704659,-2.2011435961161,-0.54695467078531));
#27323=CARTESIAN_POINT('Ctrl Pts',(93.484812286485,-0.732912553505195,-2.14639971376836));
#27324=CARTESIAN_POINT('Ctrl Pts',(93.6039630025041,1.40692946190011,-1.77897218411791));
#27325=CARTESIAN_POINT('Ctrl Pts',(93.7231137185235,2.25751908282776,0.218632415740387));
#27326=CARTESIAN_POINT('Ctrl Pts',(93.8422644345423,1.03941090339178,2.01589124618118));
#27327=CARTESIAN_POINT('Ctrl Pts',(93.9614151505618,-1.13117075273913,1.96587010524642));
#27328=CARTESIAN_POINT('Ctrl Pts',(94.0805658665806,-2.26519397362513,0.114406312735795));
#27329=CARTESIAN_POINT('Ctrl Pts',(94.1997165826001,-1.32348643932714,-1.84189472757179));
#27330=CARTESIAN_POINT('Ctrl Pts',(94.318867298619,0.831009729484381,-2.11035906235078));
#27331=CARTESIAN_POINT('Ctrl Pts',(94.4380180146384,2.22400270102766,-0.444976997566919));
#27332=CARTESIAN_POINT('Ctrl Pts',(94.5571687306571,1.57901090840168,1.62816371833129));
#27333=CARTESIAN_POINT('Ctrl Pts',(94.6763194466765,-0.512921651109511,
2.20932205039589));
#27334=CARTESIAN_POINT('Ctrl Pts',(94.7954701626955,-2.13483386860821,0.765948363785368));
#27335=CARTESIAN_POINT('Ctrl Pts',(94.9146208787147,-1.8004719789551,-1.37930895579624));
#27336=CARTESIAN_POINT('Ctrl Pts',(95.0337715947338,0.183768510093922,-2.26062417868165));
#27337=CARTESIAN_POINT('Ctrl Pts',(95.152922310753,1.99961108149091,-1.0703962188465));
#27338=CARTESIAN_POINT('Ctrl Pts',(95.2720730267721,1.98309215599787,1.10069888859847));
#27339=CARTESIAN_POINT('Ctrl Pts',(95.3912237427913,0.149348998717781,2.26315872601198));
#27340=CARTESIAN_POINT('Ctrl Pts',(95.5103744588103,-1.82125144915379,1.35175282559255));
#27341=CARTESIAN_POINT('Ctrl Pts',(95.6295251748296,-2.12293184428369,-0.79834386517865));
#27342=CARTESIAN_POINT('Ctrl Pts',(95.7486758908488,-0.479244658690441,
-2.21687101556651));
#27343=CARTESIAN_POINT('Ctrl Pts',(95.8678266068677,1.60360265574138,-1.60394858553549));
#27344=CARTESIAN_POINT('Ctrl Pts',(95.9869773228869,2.21697433569119,0.47876647483795));
#27345=CARTESIAN_POINT('Ctrl Pts',(96.106128038906,0.79880175690192,2.1227595944225));
#27346=CARTESIAN_POINT('Ctrl Pts',(96.2252787549253,-1.35135995544623,1.82154297598446));
#27347=CARTESIAN_POINT('Ctrl Pts',(96.3444294709443,-2.26319088751455,-0.148860838413323));
#27348=CARTESIAN_POINT('Ctrl Pts',(96.4635801869636,-1.10112661026953,-1.98285469228083));
#27349=CARTESIAN_POINT('Ctrl Pts',(96.5827309029826,1.06996488358556,-1.99984191636073));
#27350=CARTESIAN_POINT('Ctrl Pts',(96.7018816190017,2.26058448775406,-0.18425611595587));
#27351=CARTESIAN_POINT('Ctrl Pts',(96.8210323350211,1.3796972803395,1.80017442409833));
#27352=CARTESIAN_POINT('Ctrl Pts',(96.9401830510401,-0.765487868441268,
2.13499903180046));
#27353=CARTESIAN_POINT('Ctrl Pts',(97.0593337670593,-2.20921136327364,0.513398183602814));
#27354=CARTESIAN_POINT('Ctrl Pts',(97.1784844830784,-1.62850426857331,-1.57865968145962));
#27355=CARTESIAN_POINT('Ctrl Pts',(97.2976351990974,0.444497276236559,-2.22409862950561));
#27356=CARTESIAN_POINT('Ctrl Pts',(97.4167859151166,2.1101797668311,-0.831464908624157));
#27357=CARTESIAN_POINT('Ctrl Pts',(97.5359366311357,1.84218015697973,1.32308911732048));
#27358=CARTESIAN_POINT('Ctrl Pts',(97.6550873471549,-0.113917714318317,
2.26521859768917));
#27359=CARTESIAN_POINT('Ctrl Pts',(97.7742380631742,-1.96562606909477,1.13159475966008));
#27360=CARTESIAN_POINT('Ctrl Pts',(97.8933887791931,-2.01611539751116,-1.03897605867206));
#27361=CARTESIAN_POINT('Ctrl Pts',(98.0125394952124,-0.219119350468773,
-2.25747186912984));
#27362=CARTESIAN_POINT('Ctrl Pts',(98.1316902112315,1.77866867097777,-1.40731315392992));
#27363=CARTESIAN_POINT('Ctrl Pts',(98.2508409272507,2.14655775319236,0.732449575308886));
#27364=CARTESIAN_POINT('Ctrl Pts',(98.3699916432698,0.547429433976551,2.20102554625602));
#27365=CARTESIAN_POINT('Ctrl Pts',(98.4891423592887,-1.55334072716016,1.65267215339111));
#27366=CARTESIAN_POINT('Ctrl Pts',(98.6082930753081,-2.23069325247167,-0.41012230448011));
#27367=CARTESIAN_POINT('Ctrl Pts',(98.7274437913271,-0.863930005401265,
-2.09709720722778));
#27368=CARTESIAN_POINT('Ctrl Pts',(98.8465945073463,1.29450310557135,-1.86237895473961));
#27369=CARTESIAN_POINT('Ctrl Pts',(98.9657452233654,2.266706963286,0.0789481523067152));
#27370=CARTESIAN_POINT('Ctrl Pts',(99.0848959393846,1.16179313793426,1.94792793595931));
#27371=CARTESIAN_POINT('Ctrl Pts',(99.2040466554037,-1.00773925075854,2.03191147032719));
#27372=CARTESIAN_POINT('Ctrl Pts',(99.3231973714228,-2.25382269353839,0.253924929461906));
#27373=CARTESIAN_POINT('Ctrl Pts',(99.4423480874419,-1.43459171437324,-1.75672841829582));
#27374=CARTESIAN_POINT('Ctrl Pts',(99.561498803461,0.69923256232949,-2.15762694988174));
#27375=CARTESIAN_POINT('Ctrl Pts',(99.6806495194802,2.19232406129163,-0.581287100350585));
#27376=CARTESIAN_POINT('Ctrl Pts',(99.7998002354995,1.6764294618726,1.52756577932349));
#27377=CARTESIAN_POINT('Ctrl Pts',(99.9189509515185,-0.37561584261887,2.23692799623998));
#27378=CARTESIAN_POINT('Ctrl Pts',(100.038101667538,-2.08358259274135,0.895847985262117));
#27379=CARTESIAN_POINT('Ctrl Pts',(100.157252383557,-1.88199948336444,-1.26492822400963));
#27380=CARTESIAN_POINT('Ctrl Pts',(100.276403099576,0.0436846616069731,
-2.26902032111459));
#27381=CARTESIAN_POINT('Ctrl Pts',(100.395578889361,1.93078926426895,-1.18865410939485));
#27382=CARTESIAN_POINT('Ctrl Pts',(100.475037773807,2.00649135135404,0.250514995432669));
#27383=CARTESIAN_POINT('Ctrl Pts',(100.514779752912,1.73115616798497,0.826881453880298));
#27384=CARTESIAN_POINT('Ctrl Pts',(90.3516911588482,-1.48583601754912,0.967411654221745));
#27385=CARTESIAN_POINT('Ctrl Pts',(90.3914229117759,-1.80786151170457,0.472848642870747));
#27386=CARTESIAN_POINT('Ctrl Pts',(90.4708715700433,-1.91312324135679,-0.854610789226363));
#27387=CARTESIAN_POINT('Ctrl Pts',(90.5900371336504,-0.315584604485434,
-2.07347043422413));
#27388=CARTESIAN_POINT('Ctrl Pts',(90.7091878496695,1.57058439145835,-1.38743177376504));
#27389=CARTESIAN_POINT('Ctrl Pts',(90.8283385656886,2.01768277126442,0.567694127577208));
#27390=CARTESIAN_POINT('Ctrl Pts',(90.9474892817076,0.615787752066693,2.00375727084625));
#27391=CARTESIAN_POINT('Ctrl Pts',(91.066639997727,-1.35035406894049,1.60308306366094));
#27392=CARTESIAN_POINT('Ctrl Pts',(91.185790713746,-2.07910482788197,-0.266301222520941));
#27393=CARTESIAN_POINT('Ctrl Pts',(91.3049414297653,-0.902640265067203,
-1.89180332658395));
#27394=CARTESIAN_POINT('Ctrl Pts',(91.4240921457842,1.10096224806914,-1.78366156273085));
#27395=CARTESIAN_POINT('Ctrl Pts',(91.5432428618034,2.09569043340321,-0.0410822156528534));
#27396=CARTESIAN_POINT('Ctrl Pts',(91.6623935778227,1.17001280663651,1.73916158556239));
#27397=CARTESIAN_POINT('Ctrl Pts',(91.7815442938416,-0.827815945467298,
1.92569987629852));
#27398=CARTESIAN_POINT('Ctrl Pts',(91.9006950098609,-2.06706844074748,0.347610502843638));
#27399=CARTESIAN_POINT('Ctrl Pts',(92.0198457258799,-1.41214414015499,-1.54901719283562));
#27400=CARTESIAN_POINT('Ctrl Pts',(92.1389964418991,0.536810999374776,-2.02618796151878));
#27401=CARTESIAN_POINT('Ctrl Pts',(92.2581471579182,1.99385461541733,-0.64664385891275));
#27402=CARTESIAN_POINT('Ctrl Pts',(92.3772978739375,1.62381170543408,1.32545842158787));
#27403=CARTESIAN_POINT('Ctrl Pts',(92.4964485899565,-0.234225573255156,
2.08296487592058));
#27404=CARTESIAN_POINT('Ctrl Pts',(92.6155993059758,-1.87762815784551,0.931727912763529));
#27405=CARTESIAN_POINT('Ctrl Pts',(92.7347500219948,-1.80044938619497,-1.07330629295879));
#27406=CARTESIAN_POINT('Ctrl Pts',(92.853900738014,-0.0734127193897878,
-2.09480665988727));
#27407=CARTESIAN_POINT('Ctrl Pts',(92.9730514540332,1.72089634993666,-1.19671221974878));
#27408=CARTESIAN_POINT('Ctrl Pts',(93.0922021700523,1.93824665886355,0.798000169787126));
#27409=CARTESIAN_POINT('Ctrl Pts',(93.2113528860714,0.379467308499514,2.06145796491198));
#27410=CARTESIAN_POINT('Ctrl Pts',(93.3305036020905,-1.52704030362853,1.43588031962378));
#27411=CARTESIAN_POINT('Ctrl Pts',(93.4496543181096,-2.03423087728717,-0.505479098115718));
#27412=CARTESIAN_POINT('Ctrl Pts',(93.5688050341289,-0.67733579459438,-1.98363822353627));
#27413=CARTESIAN_POINT('Ctrl Pts',(93.6879557501479,1.3002420008455,-1.64407272344841));
#27414=CARTESIAN_POINT('Ctrl Pts',(93.8071064661672,2.08633141084316,0.202053519661223));
#27415=CARTESIAN_POINT('Ctrl Pts',(93.9262571821861,0.960592374618062,1.86302621304239));
#27416=CARTESIAN_POINT('Ctrl Pts',(94.0454078982054,-1.04539407459211,1.81679817522325));
#27417=CARTESIAN_POINT('Ctrl Pts',(94.1645586142245,-2.0934243146716,0.10573088204438));
#27418=CARTESIAN_POINT('Ctrl Pts',(94.2837093302435,-1.22312646267178,-1.70222385043407));
#27419=CARTESIAN_POINT('Ctrl Pts',(94.4028600462628,0.767994261721968,-1.95033053471462));
#27420=CARTESIAN_POINT('Ctrl Pts',(94.5220107622818,2.05535657627397,-0.411234391854458));
#27421=CARTESIAN_POINT('Ctrl Pts',(94.6411614783011,1.45927451126389,1.504700063618));
#27422=CARTESIAN_POINT('Ctrl Pts',(94.7603121943202,-0.474026802320936,
2.04178915937917));
#27423=CARTESIAN_POINT('Ctrl Pts',(94.8794629103393,-1.97294941641427,0.707866499381977));
#27424=CARTESIAN_POINT('Ctrl Pts',(94.9986136263584,-1.66394218884373,-1.27471595771868));
#27425=CARTESIAN_POINT('Ctrl Pts',(95.1177643423775,0.169833343978903,-2.08920104727853));
#27426=CARTESIAN_POINT('Ctrl Pts',(95.2369150583968,1.84798057324012,-0.989228073602758));
#27427=CARTESIAN_POINT('Ctrl Pts',(95.3560657744157,1.83271427786672,1.01723289190835));
#27428=CARTESIAN_POINT('Ctrl Pts',(95.475216490435,0.138023864149379,2.09154339988488));
#27429=CARTESIAN_POINT('Ctrl Pts',(95.5943672064542,-1.68314595181788,1.2492494088675));
#27430=CARTESIAN_POINT('Ctrl Pts',(95.7135179224733,-1.96194992259393,-0.737805449905584));
#27431=CARTESIAN_POINT('Ctrl Pts',(95.8326686384925,-0.442903536235988,
-2.04876568652113));
#27432=CARTESIAN_POINT('Ctrl Pts',(95.9518193545115,1.48200146640357,-1.48232116434138));
#27433=CARTESIAN_POINT('Ctrl Pts',(96.0709700705307,2.04886117188075,0.442461613065045));
#27434=CARTESIAN_POINT('Ctrl Pts',(96.1901207865498,0.738228619699466,1.96179073443972));
#27435=CARTESIAN_POINT('Ctrl Pts',(96.3092715025689,-1.24888633006439,1.68341537216896));
#27436=CARTESIAN_POINT('Ctrl Pts',(96.4284222185881,-2.0915731225807,-0.13757272104082));
#27437=CARTESIAN_POINT('Ctrl Pts',(96.5475729346072,-1.01762817944508,-1.83249482102335));
#27438=CARTESIAN_POINT('Ctrl Pts',(96.6667236506264,0.988829446494665,-1.84819390390174));
#27439=CARTESIAN_POINT('Ctrl Pts',(96.7858743666454,2.08916436611398,-0.170283974688326));
#27440=CARTESIAN_POINT('Ctrl Pts',(96.9050250826647,1.27507483561182,1.66366719757177));
#27441=CARTESIAN_POINT('Ctrl Pts',(97.0241757986838,-0.707440923399836,
1.97310205528165));
#27442=CARTESIAN_POINT('Ctrl Pts',(97.1433265147031,-2.0416868656614,0.474467199355257));
#27443=CARTESIAN_POINT('Ctrl Pts',(97.262477230722,-1.50501478993517,-1.45894991786086));
#27444=CARTESIAN_POINT('Ctrl Pts',(97.3816279467414,0.410791047792594,-2.05544523049543));
#27445=CARTESIAN_POINT('Ctrl Pts',(97.5007786627603,1.95016483517421,-0.768414924627563));
#27446=CARTESIAN_POINT('Ctrl Pts',(97.6199293787795,1.70248763572999,1.22275926959289));
#27447=CARTESIAN_POINT('Ctrl Pts',(97.7390800947986,-0.105279334044914,
2.09344707149284));
#27448=CARTESIAN_POINT('Ctrl Pts',(97.8582308108178,-1.81657264433298,1.04578592906823));
#27449=CARTESIAN_POINT('Ctrl Pts',(97.9773815268368,-1.86323336697702,-0.960190504173446));
#27450=CARTESIAN_POINT('Ctrl Pts',(98.0965322428562,-0.20250353012914,-2.08628777735995));
#27451=CARTESIAN_POINT('Ctrl Pts',(98.215682958875,1.64379222570971,-1.30059659750868));
#27452=CARTESIAN_POINT('Ctrl Pts',(98.3348336748945,1.98378427883073,0.676907924034713));
#27453=CARTESIAN_POINT('Ctrl Pts',(98.4539843909134,0.505917860014153,2.03412177914799));
#27454=CARTESIAN_POINT('Ctrl Pts',(98.5731351069327,-1.43555089986518,1.52735002404793));
#27455=CARTESIAN_POINT('Ctrl Pts',(98.6922858229516,-2.06153978320217,-0.379022730143428));
#27456=CARTESIAN_POINT('Ctrl Pts',(98.8114365389709,-0.798418193117015,
-1.93807432606522));
#27457=CARTESIAN_POINT('Ctrl Pts',(98.9305872549901,1.19634093511385,-1.72115475865633));
#27458=CARTESIAN_POINT('Ctrl Pts',(99.0497379710091,2.09482257432651,0.0729615139196275));
#27459=CARTESIAN_POINT('Ctrl Pts',(99.1688886870284,1.07369436431878,1.80021656063267));
#27460=CARTESIAN_POINT('Ctrl Pts',(99.2880394030473,-0.931322383403096,
1.87783162359188));
#27461=CARTESIAN_POINT('Ctrl Pts',(99.4071901190665,-2.08291531875349,0.234669802068244));
#27462=CARTESIAN_POINT('Ctrl Pts',(99.5263408350856,-1.32580662471439,-1.62351570238799));
#27463=CARTESIAN_POINT('Ctrl Pts',(99.6454915511049,0.646209757148569,-1.99401409833549));
#27464=CARTESIAN_POINT('Ctrl Pts',(99.764642267124,2.02608012778821,-0.537208099548037));
#27465=CARTESIAN_POINT('Ctrl Pts',(99.8837929831432,1.54930581582797,1.41173046632221));
#27466=CARTESIAN_POINT('Ctrl Pts',(100.002943699162,-0.347132893284113,
2.06730174635073));
#27467=CARTESIAN_POINT('Ctrl Pts',(100.122094415182,-1.92558452479489,0.827915832565954));
#27468=CARTESIAN_POINT('Ctrl Pts',(100.241245131201,-1.73928746259611,-1.1690087168201));
#27469=CARTESIAN_POINT('Ctrl Pts',(100.36039584722,0.0403720537186134,-2.09696051023103));
#27470=CARTESIAN_POINT('Ctrl Pts',(100.479571637005,1.78437751441608,-1.09851846831429));
#27471=CARTESIAN_POINT('Ctrl Pts',(100.559030521451,1.85433911223973,0.231518443336371));
#27472=CARTESIAN_POINT('Ctrl Pts',(100.598772500556,1.59988259581745,0.764179033256822));
#27473=CARTESIAN_POINT('',(100.350702918754,-0.0938353553295348,-1.775226569468));
#27474=CARTESIAN_POINT('Ctrl Pts',(100.349869898683,-0.0938337030310376,
-1.77668351508419));
#27475=CARTESIAN_POINT('Ctrl Pts',(100.349869898683,-0.0511432819576657,
-1.78421672036901));
#27476=CARTESIAN_POINT('Ctrl Pts',(100.349869898683,-0.00826292637260597,
-1.79006544278199));
#27477=CARTESIAN_POINT('Ctrl Pts',(100.349869898683,0.0347219594181997,
-1.79419129823274));
#27478=CARTESIAN_POINT('Ctrl Pts',(100.349869898683,0.0995747997289625,
-1.80041612446574));
#27479=CARTESIAN_POINT('Ctrl Pts',(100.349869898683,0.164664857862777,-1.80272216545712));
#27480=CARTESIAN_POINT('Ctrl Pts',(100.349869898683,0.229725300885458,-1.80133298954638));
#27481=CARTESIAN_POINT('Ctrl Pts',(100.349869898683,0.296581023837173,-1.79990548067148));
#27482=CARTESIAN_POINT('Ctrl Pts',(100.349869898682,0.363406212846286,-1.79457604187679));
#27483=CARTESIAN_POINT('Ctrl Pts',(100.349869898682,0.429927457817056,-1.78553511431891));
#27484=CARTESIAN_POINT('Ctrl Pts',(100.349869898682,0.46188858927035,-1.78119126485752));
#27485=CARTESIAN_POINT('Ctrl Pts',(100.349869898682,0.49377972082037,-1.7759898677578));
#27486=CARTESIAN_POINT('Ctrl Pts',(100.349869898682,0.525570989729067,-1.76994792489354));
#27487=CARTESIAN_POINT('Ctrl Pts',(100.349869898682,0.544239449495205,-1.76639997694611));
#27488=CARTESIAN_POINT('Ctrl Pts',(100.349869898682,0.562873475889264,-1.76256213670098));
#27489=CARTESIAN_POINT('Ctrl Pts',(100.349869898682,0.581467005198649,-1.75843743329571));
#27490=CARTESIAN_POINT('Ctrl Pts',(100.349869898682,0.596154585183419,-1.75517920780392));
#27491=CARTESIAN_POINT('Ctrl Pts',(100.349869898682,0.610820358907282,-1.75174098890037));
#27492=CARTESIAN_POINT('Ctrl Pts',(100.349869898682,0.625435174434094,-1.74813099328831));
#27493=CARTESIAN_POINT('Ctrl Pts',(100.349869898682,0.693327091226846,-1.73136105724182));
#27494=CARTESIAN_POINT('Ctrl Pts',(100.349869898682,0.760228106371345,-1.71086602232306));
#27495=CARTESIAN_POINT('Ctrl Pts',(100.349869898682,0.825842051564602,-1.68688364802346));
#27496=CARTESIAN_POINT('Ctrl Pts',(100.349869898682,0.892658275793112,-1.66246183199006));
#27497=CARTESIAN_POINT('Ctrl Pts',(100.349869898682,0.958140785980623,-1.63442357221684));
#27498=CARTESIAN_POINT('Ctrl Pts',(100.349869898682,1.02198275116856,-1.60296574252318));
#27499=CARTESIAN_POINT('Ctrl Pts',(100.349869898682,1.08621375452109,-1.57131621609384));
#27500=CARTESIAN_POINT('Ctrl Pts',(100.349869898682,1.1487852181858,-1.53620505098691));
#27501=CARTESIAN_POINT('Ctrl Pts',(100.349869898682,1.20937529811015,-1.49778156541698));
#27502=CARTESIAN_POINT('Ctrl Pts',(100.349869898682,1.22829221885182,-1.48578531071566));
#27503=CARTESIAN_POINT('Ctrl Pts',(100.349869898682,1.24701586973985,-1.47346582697558));
#27504=CARTESIAN_POINT('Ctrl Pts',(100.349869898682,1.26553601308475,-1.46082671008806));
#27505=CARTESIAN_POINT('Ctrl Pts',(100.349869898682,1.27472938384671,-1.45455267184294));
#27506=CARTESIAN_POINT('Ctrl Pts',(100.349869898682,1.28386964618851,-1.44820182666929));
#27507=CARTESIAN_POINT('Ctrl Pts',(100.349869898682,1.29294880238582,-1.44177972141044));
#27508=CARTESIAN_POINT('Ctrl Pts',(100.349869898682,1.35324423932221,-1.39912998235782));
#27509=CARTESIAN_POINT('Ctrl Pts',(100.349869898682,1.41093556061047,-1.35328021416844));
#27510=CARTESIAN_POINT('Ctrl Pts',(100.349869898682,1.4657028486192,-1.30444825214604));
#27511=CARTESIAN_POINT('Ctrl Pts',(100.349869898682,1.52027452528291,-1.25579070237076));
#27512=CARTESIAN_POINT('Ctrl Pts',(100.349869898682,1.57194408047454,-1.20417182309451));
#27513=CARTESIAN_POINT('Ctrl Pts',(100.349869898682,1.62038013382389,-1.14975844237987));
#27514=CARTESIAN_POINT('Ctrl Pts',(100.349869898682,1.64885755147716,-1.11776672419916));
#27515=CARTESIAN_POINT('Ctrl Pts',(100.349869898682,1.67621688120137,-1.08480813775943));
#27516=CARTESIAN_POINT('Ctrl Pts',(100.349869898682,1.70238609206081,-1.05090953536274));
#27517=CARTESIAN_POINT('Ctrl Pts',(100.349869898682,1.73605338905434,-1.00729819680594));
#27518=CARTESIAN_POINT('Ctrl Pts',(100.349869898682,1.76775143347145,-0.962131310211133));
#27519=CARTESIAN_POINT('Ctrl Pts',(100.349869898682,1.79747650045091,-0.915546859126332));
#27520=CARTESIAN_POINT('Ctrl Pts',(100.349869898682,1.80400780711809,-0.905311143386221));
#27521=CARTESIAN_POINT('Ctrl Pts',(100.349869898682,1.81043884326659,-0.895014695114994));
#27522=CARTESIAN_POINT('Ctrl Pts',(100.349869898682,1.81676859411663,-0.88466146049614));
#27523=CARTESIAN_POINT('Ctrl Pts',(100.349869898683,1.85447403403412,-0.822988690884629));
#27524=CARTESIAN_POINT('Ctrl Pts',(100.349869898683,1.88860369126805,-0.759280016585824));
#27525=CARTESIAN_POINT('Ctrl Pts',(100.349869898683,1.91920882291116,-0.69389751131988));
#27526=CARTESIAN_POINT('Ctrl Pts',(100.349869898683,1.95083266173162,-0.626338716529564));
#27527=CARTESIAN_POINT('Ctrl Pts',(100.349869898683,1.97869389269075,-0.556992193784614));
#27528=CARTESIAN_POINT('Ctrl Pts',(100.349869898683,2.0028101728334,-0.486216002267792));
#27529=CARTESIAN_POINT('Ctrl Pts',(100.349869898683,2.02692645297605,-0.41543981075097));
#27530=CARTESIAN_POINT('Ctrl Pts',(100.349869898683,2.04729804958241,-0.343233053659112));
#27531=CARTESIAN_POINT('Ctrl Pts',(100.349869898683,2.063899203451,-0.269924895638601));
#27532=CARTESIAN_POINT('Ctrl Pts',(100.349869898683,2.06724025486579,-0.255171323265941));
#27533=CARTESIAN_POINT('Ctrl Pts',(100.349869898683,2.07042844291423,-0.240373072421456));
#27534=CARTESIAN_POINT('Ctrl Pts',(100.349869898683,2.07346332984018,-0.225532735420184));
#27535=CARTESIAN_POINT('Ctrl Pts',(100.349869898683,2.07629732325745,-0.211674750461333));
#27536=CARTESIAN_POINT('Ctrl Pts',(100.349869898683,2.07899763861497,-0.197780066263633));
#27537=CARTESIAN_POINT('Ctrl Pts',(100.349869898683,2.08156385697044,-0.183850777551013));
#27538=CARTESIAN_POINT('Ctrl Pts',(100.349869898683,2.08418234040355,-0.169637796940397));
#27539=CARTESIAN_POINT('Ctrl Pts',(100.349869898683,2.08665986231528,-0.155395799266699));
#27540=CARTESIAN_POINT('Ctrl Pts',(100.349869898683,2.08899516018126,-0.141135229261509));
#27541=CARTESIAN_POINT('Ctrl Pts',(100.349869898683,2.10161552092171,-0.0640685987247987));
#27542=CARTESIAN_POINT('Ctrl Pts',(100.349869898683,2.11009928121374,0.0136100998382424));
#27543=CARTESIAN_POINT('Ctrl Pts',(100.349869898683,2.11445263267422,0.0915223436362172));
#27544=CARTESIAN_POINT('Ctrl Pts',(100.349869898683,2.11878556589602,0.169069160749906));
#27545=CARTESIAN_POINT('Ctrl Pts',(100.349869898683,2.1190269676162,0.246848345957318));
#27546=CARTESIAN_POINT('Ctrl Pts',(100.349869898682,2.11513535441828,0.324505766001828));
#27547=CARTESIAN_POINT('Ctrl Pts',(100.349869898682,2.11414398385978,0.344288636489222));
#27548=CARTESIAN_POINT('Ctrl Pts',(100.349869898682,2.11288414907951,0.364063658710047));
#27549=CARTESIAN_POINT('Ctrl Pts',(100.349869898682,2.11135463994554,0.383825055241067));
#27550=CARTESIAN_POINT('Ctrl Pts',(100.349869898682,2.11020352169258,0.398697607320445));
#27551=CARTESIAN_POINT('Ctrl Pts',(100.349869898682,2.10890040119927,0.41355265810877));
#27552=CARTESIAN_POINT('Ctrl Pts',(100.349869898682,2.10744539990257,0.428386817866786));
#27553=CARTESIAN_POINT('Ctrl Pts',(100.349869898682,2.09968291124935,0.507527638608771));
#27554=CARTESIAN_POINT('Ctrl Pts',(100.349869898682,2.08760086541998,0.586080887221537));
#27555=CARTESIAN_POINT('Ctrl Pts',(100.349869898682,2.07117840522959,0.663672733754418));
#27556=CARTESIAN_POINT('Ctrl Pts',(100.349869898682,2.05490267436401,0.740571322448959));
#27557=CARTESIAN_POINT('Ctrl Pts',(100.349869898682,2.03436391310342,0.816526640045261));
#27558=CARTESIAN_POINT('Ctrl Pts',(100.349869898682,2.00949149356056,0.891179159993276));
#27559=CARTESIAN_POINT('Ctrl Pts',(100.349869898682,2.00307587526026,0.910435110236372));
#27560=CARTESIAN_POINT('Ctrl Pts',(100.349869898682,1.99637165302191,0.929604358635672));
#27561=CARTESIAN_POINT('Ctrl Pts',(100.349869898682,1.98937704260631,0.948680653513866));
#27562=CARTESIAN_POINT('Ctrl Pts',(100.349869898682,-0.11727379276914,-1.77237437355361));
#27563=CARTESIAN_POINT('Ctrl Pts',(100.350147572039,-0.109438590926001,
-1.77289281020614));
#27564=CARTESIAN_POINT('Ctrl Pts',(100.350425245396,-0.101599951227993,
-1.77335929004107));
#27565=CARTESIAN_POINT('Ctrl Pts',(100.350702918754,-0.0937585630115176,
-1.77377377203577));
#27566=CARTESIAN_POINT('Origin',(100.349869898682,0.,0.));
#27567=CARTESIAN_POINT('Origin',(33.1926516271063,0.,0.));
#27568=CARTESIAN_POINT('',(33.4926516271063,-5.13007994755883E-16,4.18902817623056));
#27569=CARTESIAN_POINT('Origin',(33.4926516271063,0.,0.));
#27570=CARTESIAN_POINT('',(33.1926516271063,-5.49747398730303E-16,4.48902817623056));
#27571=CARTESIAN_POINT('Origin',(33.1926516271063,-5.13007994755883E-16,
4.18902817623056));
#27572=CARTESIAN_POINT('Origin',(33.1926516271063,0.,0.));
#27573=CARTESIAN_POINT('Origin',(32.5726008112287,0.,0.));
#27574=CARTESIAN_POINT('',(31.6525499953511,-5.49747398730303E-16,4.48902817623056));
#27575=CARTESIAN_POINT('',(32.5726008112287,-5.49747398730304E-16,4.48902817623056));
#27576=CARTESIAN_POINT('Origin',(31.6525499953511,0.,0.));
#27577=CARTESIAN_POINT('Origin',(33.4926516271063,0.,-2.21164758166987));
#27578=CARTESIAN_POINT('Origin',(31.3525499953512,0.,0.));
#27579=CARTESIAN_POINT('',(31.6525499953511,-7.4821050118432E-16,6.1096023907077));
#27580=CARTESIAN_POINT('Origin',(31.6525499953511,0.,0.));
#27581=CARTESIAN_POINT('',(31.3524613125654,-7.84949903553507E-16,6.40960237759997));
#27582=CARTESIAN_POINT('Origin',(31.3525499953512,-7.4821050118432E-16,
6.1096023907077));
#27583=CARTESIAN_POINT('Origin',(31.3524613125654,-7.84949903553507E-16,
0.));
#27584=CARTESIAN_POINT('Origin',(31.0318089645314,0.,0.));
#27585=CARTESIAN_POINT('',(30.7109792509259,-7.84926680813535E-16,6.40941274953751));
#27586=CARTESIAN_POINT('',(31.0318089645314,-7.84938295393988E-16,6.40950758978419));
#27587=CARTESIAN_POINT('Origin',(30.7109792509259,-7.84926680813535E-16,
0.));
#27588=CARTESIAN_POINT('Origin',(31.6525499953511,0.,-4.48902817623056));
#27589=CARTESIAN_POINT('Origin',(30.7110679337117,0.,0.));
#27590=CARTESIAN_POINT('',(30.4110679337117,-7.48187278444348E-16,6.10941276264524));
#27591=CARTESIAN_POINT('Origin',(30.7110679337117,-7.48187278444348E-16,
6.10941276264524));
#27592=CARTESIAN_POINT('Origin',(30.4110679337117,0.,0.));
#27593=CARTESIAN_POINT('Origin',(30.4110679337117,0.,-6.40932409296331));
#27594=CARTESIAN_POINT('',(30.4110679337117,-2.70848713173399E-16,2.21164758166987));
#27595=CARTESIAN_POINT('Origin',(30.4110679337117,0.,0.));
#27596=CARTESIAN_POINT('Origin',(28.3729800631879,0.,0.));
#27597=CARTESIAN_POINT('',(28.6729800631879,-7.48102635692981E-16,6.1087216021292));
#27598=CARTESIAN_POINT('Origin',(28.6729800631879,0.,0.));
#27599=CARTESIAN_POINT('',(28.3728913804021,-7.84842038062168E-16,6.40872158902147));
#27600=CARTESIAN_POINT('Origin',(28.3729800631879,-7.48102635692982E-16,
6.1087216021292));
#27601=CARTESIAN_POINT('Origin',(28.3728913804021,-7.84842038062168E-16,
0.));
#27602=CARTESIAN_POINT('Origin',(28.2136282688352,0.,0.));
#27603=CARTESIAN_POINT('',(28.0541877916966,-7.84830500451046E-16,6.40862737727707));
#27604=CARTESIAN_POINT('',(28.2136282688352,-7.84836272467075E-16,6.40867450936473));
#27605=CARTESIAN_POINT('Origin',(28.0541877916966,-7.84830500451046E-16,
0.));
#27606=CARTESIAN_POINT('Origin',(28.6729800631879,0.,0.));
#27607=CARTESIAN_POINT('',(28.6729800631879,-2.70848713173399E-16,2.21164758166987));
#27608=CARTESIAN_POINT('Origin',(28.6729800631879,0.,0.));
#27609=CARTESIAN_POINT('Origin',(28.0542764744824,0.,0.));
#27610=CARTESIAN_POINT('Origin',(28.0542764744824,-7.4809109808186E-16,
6.1086273903848));
#27611=CARTESIAN_POINT('Origin',(25.1947388265965,0.,0.));
#27612=CARTESIAN_POINT('',(25.1946501438108,-7.84726980332233E-16,6.40778207135796));
#27613=CARTESIAN_POINT('Origin',(25.1947388265965,-7.47987577963046E-16,
6.10778208446569));
#27614=CARTESIAN_POINT('Origin',(25.1946501438108,-7.84726980332233E-16,
0.));
#27615=CARTESIAN_POINT('Origin',(25.0105689136245,0.,0.));
#27616=CARTESIAN_POINT('',(24.8263103178667,-7.84713645805033E-16,6.40767318668028));
#27617=CARTESIAN_POINT('',(25.0105689136245,-7.847203162791E-16,6.40772765523458));
#27618=CARTESIAN_POINT('Origin',(24.8263103178667,-7.84713645805033E-16,
0.));
#27619=CARTESIAN_POINT('Origin',(24.8263990006525,0.,0.));
#27620=CARTESIAN_POINT('',(24.5263990006525,-7.47974243435846E-16,6.10767319978801));
#27621=CARTESIAN_POINT('Origin',(24.8263990006525,-7.47974243435846E-16,
6.10767319978801));
#27622=CARTESIAN_POINT('Origin',(24.5263990006525,0.,0.));
#27623=CARTESIAN_POINT('Origin',(24.5263990006525,0.,-6.40758453010608));
#27624=CARTESIAN_POINT('',(24.5263990006525,-2.70848713173399E-16,2.21164758166987));
#27625=CARTESIAN_POINT('Origin',(24.5263990006525,0.,0.));
#27626=CARTESIAN_POINT('Origin',(22.4730782633311,0.,0.));
#27627=CARTESIAN_POINT('',(22.7730782633312,-7.47889049228833E-16,6.1069775362949));
#27628=CARTESIAN_POINT('Origin',(22.7730782633312,0.,0.));
#27629=CARTESIAN_POINT('',(22.4729895805454,-7.8462845159802E-16,6.40697752318717));
#27630=CARTESIAN_POINT('Origin',(22.4730782633311,-7.47889049228834E-16,
6.1069775362949));
#27631=CARTESIAN_POINT('Origin',(22.4729895805454,-7.8462845159802E-16,
0.));
#27632=CARTESIAN_POINT('Origin',(22.2310089528171,0.,0.));
#27633=CARTESIAN_POINT('',(21.9888509595172,-7.84610924957793E-16,6.40683440730886));
#27634=CARTESIAN_POINT('',(22.2310089528171,-7.84619691488374E-16,6.40690599146347));
#27635=CARTESIAN_POINT('Origin',(21.9888509595172,-7.84610924957793E-16,
0.));
#27636=CARTESIAN_POINT('Origin',(22.7730782633312,0.,-2.21164758166987));
#27637=CARTESIAN_POINT('',(22.7730782633312,-2.70848713173399E-16,2.21164758166987));
#27638=CARTESIAN_POINT('Origin',(22.7730782633312,0.,0.));
#27639=CARTESIAN_POINT('Origin',(21.9889396423029,0.,0.));
#27640=CARTESIAN_POINT('',(21.688939642303,-7.47871522588606E-16,6.10683442041659));
#27641=CARTESIAN_POINT('Origin',(21.9889396423029,-7.47871522588606E-16,
6.10683442041659));
#27642=CARTESIAN_POINT('Origin',(21.688939642303,0.,0.));
#27643=CARTESIAN_POINT('Origin',(21.688939642303,0.,-6.40674575073467));
#27644=CARTESIAN_POINT('',(21.688939642303,-5.41697426346798E-16,4.42329516333974));
#27645=CARTESIAN_POINT('Origin',(21.688939642303,0.,0.));
#27646=CARTESIAN_POINT('Origin',(21.1989257366328,0.,0.));
#27647=CARTESIAN_POINT('',(21.1989257366328,-5.41697426346798E-16,4.42329516333974));
#27648=CARTESIAN_POINT('Origin',(21.1989257366328,0.,0.));
#27649=CARTESIAN_POINT('',(20.8989257366328,-5.04958022372377E-16,4.12329516333974));
#27650=CARTESIAN_POINT('Origin',(21.1989257366328,-5.04958022372377E-16,
4.12329516333974));
#27651=CARTESIAN_POINT('Origin',(20.8989257366328,0.,0.));
#27652=CARTESIAN_POINT('Origin',(20.8989257366328,0.,-4.42329516333974));
#27653=CARTESIAN_POINT('Origin',(21.2939326894679,0.,0.));
#27654=CARTESIAN_POINT('',(21.2939326894679,-5.41697426346798E-16,4.42329516333974));
#27655=CARTESIAN_POINT('Origin',(23.6497386319918,0.,0.));
#27656=CARTESIAN_POINT('',(23.6497386319918,-2.70848713173399E-16,2.21164758166987));
#27657=CARTESIAN_POINT('Origin',(29.5420239984498,0.,0.));
#27658=CARTESIAN_POINT('',(29.5420239984498,-2.70848713173399E-16,2.21164758166987));
#27659=CARTESIAN_POINT('',(0.,0.,0.));
#27660=CARTESIAN_POINT('Origin',(80.44,0.,0.));
#27661=CARTESIAN_POINT('',(81.44,-3.7,-4.53119315684521E-16));
#27662=CARTESIAN_POINT('Origin',(81.44,0.,0.));
#27663=CARTESIAN_POINT('',(79.44,-3.7,-4.53119315684521E-16));
#27664=CARTESIAN_POINT('',(80.44,-3.7,-4.53119315684521E-16));
#27665=CARTESIAN_POINT('Origin',(79.44,0.,0.));
#27666=CARTESIAN_POINT('Origin',(81.44,2.204,0.));
#27667=CARTESIAN_POINT('',(81.44,-2.204,-2.69912154532077E-16));
#27668=CARTESIAN_POINT('Origin',(81.44,0.,0.));
#27669=CARTESIAN_POINT('Origin',(80.44,0.,0.));
#27670=CARTESIAN_POINT('',(79.44,-2.204,-2.69912154532077E-16));
#27671=CARTESIAN_POINT('Origin',(79.44,0.,0.));
#27672=CARTESIAN_POINT('',(80.44,-2.204,-2.69912154532077E-16));
#27673=CARTESIAN_POINT('Origin',(79.44,3.7,0.));
#27674=CARTESIAN_POINT('',(0.,0.,0.));
#27675=CARTESIAN_POINT('',(0.,0.,0.));
#27676=CARTESIAN_POINT('',(0.,0.,0.));
#27677=CARTESIAN_POINT('',(0.,0.,0.));
#27678=CARTESIAN_POINT('',(0.,0.,0.));
#27679=CARTESIAN_POINT('',(0.,0.,0.));
#27680=CARTESIAN_POINT('',(0.,0.,0.));
#27681=CARTESIAN_POINT('',(0.,0.,0.));
#27682=CARTESIAN_POINT('',(0.,0.,0.));
#27683=CARTESIAN_POINT('',(0.,0.,0.));
#27684=UNCERTAINTY_MEASURE_WITH_UNIT(LENGTH_MEASURE(0.01),#27708,
'DISTANCE_ACCURACY_VALUE',
'Maximum model space distance between geometric entities at asserted c
onnectivities');
#27685=UNCERTAINTY_MEASURE_WITH_UNIT(LENGTH_MEASURE(0.01),#27708,
'DISTANCE_ACCURACY_VALUE',
'Maximum model space distance between geometric entities at asserted c
onnectivities');
#27686=UNCERTAINTY_MEASURE_WITH_UNIT(LENGTH_MEASURE(0.01),#27708,
'DISTANCE_ACCURACY_VALUE',
'Maximum model space distance between geometric entities at asserted c
onnectivities');
#27687=UNCERTAINTY_MEASURE_WITH_UNIT(LENGTH_MEASURE(0.01),#27708,
'DISTANCE_ACCURACY_VALUE',
'Maximum model space distance between geometric entities at asserted c
onnectivities');
#27688=UNCERTAINTY_MEASURE_WITH_UNIT(LENGTH_MEASURE(0.01),#27708,
'DISTANCE_ACCURACY_VALUE',
'Maximum model space distance between geometric entities at asserted c
onnectivities');
#27689=UNCERTAINTY_MEASURE_WITH_UNIT(LENGTH_MEASURE(0.01),#27708,
'DISTANCE_ACCURACY_VALUE',
'Maximum model space distance between geometric entities at asserted c
onnectivities');
#27690=UNCERTAINTY_MEASURE_WITH_UNIT(LENGTH_MEASURE(0.01),#27708,
'DISTANCE_ACCURACY_VALUE',
'Maximum model space distance between geometric entities at asserted c
onnectivities');
#27691=UNCERTAINTY_MEASURE_WITH_UNIT(LENGTH_MEASURE(0.01),#27708,
'DISTANCE_ACCURACY_VALUE',
'Maximum model space distance between geometric entities at asserted c
onnectivities');
#27692=UNCERTAINTY_MEASURE_WITH_UNIT(LENGTH_MEASURE(0.01),#27708,
'DISTANCE_ACCURACY_VALUE',
'Maximum model space distance between geometric entities at asserted c
onnectivities');
#27693=UNCERTAINTY_MEASURE_WITH_UNIT(LENGTH_MEASURE(0.01),#27708,
'DISTANCE_ACCURACY_VALUE',
'Maximum model space distance between geometric entities at asserted c
onnectivities');
#27694=UNCERTAINTY_MEASURE_WITH_UNIT(LENGTH_MEASURE(0.01),#27708,
'DISTANCE_ACCURACY_VALUE',
'Maximum model space distance between geometric entities at asserted c
onnectivities');
#27695=UNCERTAINTY_MEASURE_WITH_UNIT(LENGTH_MEASURE(0.01),#27708,
'DISTANCE_ACCURACY_VALUE',
'Maximum model space distance between geometric entities at asserted c
onnectivities');
#27696=(
GEOMETRIC_REPRESENTATION_CONTEXT(3)
GLOBAL_UNCERTAINTY_ASSIGNED_CONTEXT((#27684))
GLOBAL_UNIT_ASSIGNED_CONTEXT((#27708,#27710,#27711))
REPRESENTATION_CONTEXT('','3D')
);
#27697=(
GEOMETRIC_REPRESENTATION_CONTEXT(3)
GLOBAL_UNCERTAINTY_ASSIGNED_CONTEXT((#27685))
GLOBAL_UNIT_ASSIGNED_CONTEXT((#27708,#27710,#27711))
REPRESENTATION_CONTEXT('','3D')
);
#27698=(
GEOMETRIC_REPRESENTATION_CONTEXT(3)
GLOBAL_UNCERTAINTY_ASSIGNED_CONTEXT((#27686))
GLOBAL_UNIT_ASSIGNED_CONTEXT((#27708,#27710,#27711))
REPRESENTATION_CONTEXT('','3D')
);
#27699=(
GEOMETRIC_REPRESENTATION_CONTEXT(3)
GLOBAL_UNCERTAINTY_ASSIGNED_CONTEXT((#27687))
GLOBAL_UNIT_ASSIGNED_CONTEXT((#27708,#27710,#27711))
REPRESENTATION_CONTEXT('','3D')
);
#27700=(
GEOMETRIC_REPRESENTATION_CONTEXT(3)
GLOBAL_UNCERTAINTY_ASSIGNED_CONTEXT((#27688))
GLOBAL_UNIT_ASSIGNED_CONTEXT((#27708,#27710,#27711))
REPRESENTATION_CONTEXT('','3D')
);
#27701=(
GEOMETRIC_REPRESENTATION_CONTEXT(3)
GLOBAL_UNCERTAINTY_ASSIGNED_CONTEXT((#27689))
GLOBAL_UNIT_ASSIGNED_CONTEXT((#27708,#27710,#27711))
REPRESENTATION_CONTEXT('','3D')
);
#27702=(
GEOMETRIC_REPRESENTATION_CONTEXT(3)
GLOBAL_UNCERTAINTY_ASSIGNED_CONTEXT((#27690))
GLOBAL_UNIT_ASSIGNED_CONTEXT((#27708,#27710,#27711))
REPRESENTATION_CONTEXT('','3D')
);
#27703=(
GEOMETRIC_REPRESENTATION_CONTEXT(3)
GLOBAL_UNCERTAINTY_ASSIGNED_CONTEXT((#27691))
GLOBAL_UNIT_ASSIGNED_CONTEXT((#27708,#27710,#27711))
REPRESENTATION_CONTEXT('','3D')
);
#27704=(
GEOMETRIC_REPRESENTATION_CONTEXT(3)
GLOBAL_UNCERTAINTY_ASSIGNED_CONTEXT((#27692))
GLOBAL_UNIT_ASSIGNED_CONTEXT((#27708,#27710,#27711))
REPRESENTATION_CONTEXT('','3D')
);
#27705=(
GEOMETRIC_REPRESENTATION_CONTEXT(3)
GLOBAL_UNCERTAINTY_ASSIGNED_CONTEXT((#27693))
GLOBAL_UNIT_ASSIGNED_CONTEXT((#27708,#27710,#27711))
REPRESENTATION_CONTEXT('','3D')
);
#27706=(
GEOMETRIC_REPRESENTATION_CONTEXT(3)
GLOBAL_UNCERTAINTY_ASSIGNED_CONTEXT((#27694))
GLOBAL_UNIT_ASSIGNED_CONTEXT((#27708,#27710,#27711))
REPRESENTATION_CONTEXT('','3D')
);
#27707=(
GEOMETRIC_REPRESENTATION_CONTEXT(3)
GLOBAL_UNCERTAINTY_ASSIGNED_CONTEXT((#27695))
GLOBAL_UNIT_ASSIGNED_CONTEXT((#27708,#27710,#27711))
REPRESENTATION_CONTEXT('','3D')
);
#27708=(
LENGTH_UNIT()
NAMED_UNIT(*)
SI_UNIT(.MILLI.,.METRE.)
);
#27709=(
LENGTH_UNIT()
NAMED_UNIT(*)
SI_UNIT($,.METRE.)
);
#27710=(
NAMED_UNIT(*)
PLANE_ANGLE_UNIT()
SI_UNIT($,.RADIAN.)
);
#27711=(
NAMED_UNIT(*)
SI_UNIT($,.STERADIAN.)
SOLID_ANGLE_UNIT()
);
#27712=SHAPE_DEFINITION_REPRESENTATION(#27723,#27744);
#27713=SHAPE_DEFINITION_REPRESENTATION(#27724,#27745);
#27714=SHAPE_DEFINITION_REPRESENTATION(#27725,#27746);
#27715=SHAPE_DEFINITION_REPRESENTATION(#27726,#27747);
#27716=SHAPE_DEFINITION_REPRESENTATION(#27727,#27748);
#27717=SHAPE_DEFINITION_REPRESENTATION(#27728,#27749);
#27718=SHAPE_DEFINITION_REPRESENTATION(#27729,#27750);
#27719=SHAPE_DEFINITION_REPRESENTATION(#27730,#27751);
#27720=SHAPE_DEFINITION_REPRESENTATION(#27731,#27752);
#27721=SHAPE_DEFINITION_REPRESENTATION(#27732,#27753);
#27722=SHAPE_DEFINITION_REPRESENTATION(#27733,#27754);
#27723=PRODUCT_DEFINITION_SHAPE('',$,#27756);
#27724=PRODUCT_DEFINITION_SHAPE('',$,#27757);
#27725=PRODUCT_DEFINITION_SHAPE('',$,#27758);
#27726=PRODUCT_DEFINITION_SHAPE('',$,#27759);
#27727=PRODUCT_DEFINITION_SHAPE('',$,#27760);
#27728=PRODUCT_DEFINITION_SHAPE('',$,#27761);
#27729=PRODUCT_DEFINITION_SHAPE('',$,#27762);
#27730=PRODUCT_DEFINITION_SHAPE('',$,#27763);
#27731=PRODUCT_DEFINITION_SHAPE('',$,#27764);
#27732=PRODUCT_DEFINITION_SHAPE('',$,#27765);
#27733=PRODUCT_DEFINITION_SHAPE('',$,#27766);
#27734=PRODUCT_DEFINITION_SHAPE($,$,#41);
#27735=PRODUCT_DEFINITION_SHAPE($,$,#42);
#27736=PRODUCT_DEFINITION_SHAPE($,$,#43);
#27737=PRODUCT_DEFINITION_SHAPE($,$,#44);
#27738=PRODUCT_DEFINITION_SHAPE($,$,#45);
#27739=PRODUCT_DEFINITION_SHAPE($,$,#46);
#27740=PRODUCT_DEFINITION_SHAPE($,$,#47);
#27741=PRODUCT_DEFINITION_SHAPE($,$,#48);
#27742=PRODUCT_DEFINITION_SHAPE($,$,#49);
#27743=PRODUCT_DEFINITION_SHAPE($,$,#50);
#27744=SHAPE_REPRESENTATION('',(#3955,#4278,#4279,#4280,#4281,#4282,#4283,
#4284,#4285,#4286,#4287),#27696);
#27745=SHAPE_REPRESENTATION('',(#3956),#27697);
#27746=SHAPE_REPRESENTATION('',(#3971),#27698);
#27747=SHAPE_REPRESENTATION('',(#3993),#27699);
#27748=SHAPE_REPRESENTATION('',(#4008),#27700);
#27749=SHAPE_REPRESENTATION('',(#4052),#27701);
#27750=SHAPE_REPRESENTATION('',(#4064),#27702);
#27751=SHAPE_REPRESENTATION('',(#4092),#27703);
#27752=SHAPE_REPRESENTATION('',(#4144),#27704);
#27753=SHAPE_REPRESENTATION('',(#4156),#27705);
#27754=SHAPE_REPRESENTATION('',(#4269),#27706);
#27755=PRODUCT_DEFINITION_CONTEXT('part definition',#27790,'design');
#27756=PRODUCT_DEFINITION('BR-314_Double_Acting','BR-314',#27767,#27755);
#27757=PRODUCT_DEFINITION('Nut_01','Nut_01',#27768,#27755);
#27758=PRODUCT_DEFINITION('spacer','Spacer',#27769,#27755);
#27759=PRODUCT_DEFINITION('Nut_02','Nut_02',#27770,#27755);
#27760=PRODUCT_DEFINITION('Screw_02','Screw_02',#27771,#27755);
#27761=PRODUCT_DEFINITION('Ring_01','Ring_01',#27772,#27755);
#27762=PRODUCT_DEFINITION('Screw','Screw',#27773,#27755);
#27763=PRODUCT_DEFINITION('Cylinder','Cylinder',#27774,#27755);
#27764=PRODUCT_DEFINITION('Ring_02','Ring_02',#27775,#27755);
#27765=PRODUCT_DEFINITION('Shaft','Shaft',#27776,#27755);
#27766=PRODUCT_DEFINITION('2026-10-01-22-51-42-851','Rod_Seal',#27777,#27755);
#27767=PRODUCT_DEFINITION_FORMATION('',$,#27792);
#27768=PRODUCT_DEFINITION_FORMATION('',$,#27793);
#27769=PRODUCT_DEFINITION_FORMATION('',$,#27794);
#27770=PRODUCT_DEFINITION_FORMATION('',$,#27795);
#27771=PRODUCT_DEFINITION_FORMATION('',$,#27796);
#27772=PRODUCT_DEFINITION_FORMATION('',$,#27797);
#27773=PRODUCT_DEFINITION_FORMATION('',$,#27798);
#27774=PRODUCT_DEFINITION_FORMATION('',$,#27799);
#27775=PRODUCT_DEFINITION_FORMATION('',$,#27800);
#27776=PRODUCT_DEFINITION_FORMATION('',$,#27801);
#27777=PRODUCT_DEFINITION_FORMATION('',$,#27802);
#27778=PRODUCT_RELATED_PRODUCT_CATEGORY('BR-314','BR-314',(#27792));
#27779=PRODUCT_RELATED_PRODUCT_CATEGORY('Nut_01','Nut_01',(#27793));
#27780=PRODUCT_RELATED_PRODUCT_CATEGORY('Spacer','Spacer',(#27794));
#27781=PRODUCT_RELATED_PRODUCT_CATEGORY('Nut_02','Nut_02',(#27795));
#27782=PRODUCT_RELATED_PRODUCT_CATEGORY('Screw_02','Screw_02',(#27796));
#27783=PRODUCT_RELATED_PRODUCT_CATEGORY('Ring_01','Ring_01',(#27797));
#27784=PRODUCT_RELATED_PRODUCT_CATEGORY('Screw','Screw',(#27798));
#27785=PRODUCT_RELATED_PRODUCT_CATEGORY('Cylinder','Cylinder',(#27799));
#27786=PRODUCT_RELATED_PRODUCT_CATEGORY('Ring_02','Ring_02',(#27800));
#27787=PRODUCT_RELATED_PRODUCT_CATEGORY('Shaft','Shaft',(#27801));
#27788=PRODUCT_RELATED_PRODUCT_CATEGORY('Rod_Seal','Rod_Seal',(#27802));
#27789=APPLICATION_PROTOCOL_DEFINITION('international standard',
'automotive_design',2009,#27790);
#27790=APPLICATION_CONTEXT(
'Core Data for Automotive Mechanical Design Process');
#27791=PRODUCT_CONTEXT('part definition',#27790,'mechanical');
#27792=PRODUCT('BR-314_Double_Acting','BR-314',$,(#27791));
#27793=PRODUCT('Nut_01','Nut_01',$,(#27791));
#27794=PRODUCT('spacer','Spacer',$,(#27791));
#27795=PRODUCT('Nut_02','Nut_02',$,(#27791));
#27796=PRODUCT('Screw_02','Screw_02',$,(#27791));
#27797=PRODUCT('Ring_01','Ring_01',$,(#27791));
#27798=PRODUCT('Screw','Screw',$,(#27791));
#27799=PRODUCT('Cylinder','Cylinder',$,(#27791));
#27800=PRODUCT('Ring_02','Ring_02',$,(#27791));
#27801=PRODUCT('Shaft','Shaft',$,(#27791));
#27802=PRODUCT('2026-10-01-22-51-42-851','Rod_Seal',$,(#27791));
#27803=PRESENTATION_STYLE_ASSIGNMENT((#27805));
#27804=PRESENTATION_STYLE_ASSIGNMENT((#27806));
#27805=SURFACE_STYLE_USAGE(.BOTH.,#27807);
#27806=SURFACE_STYLE_USAGE(.BOTH.,#27808);
#27807=SURFACE_SIDE_STYLE('',(#27809));
#27808=SURFACE_SIDE_STYLE('',(#27810));
#27809=SURFACE_STYLE_FILL_AREA(#27811);
#27810=SURFACE_STYLE_FILL_AREA(#27812);
#27811=FILL_AREA_STYLE('Steel - Satin',(#27813));
#27812=FILL_AREA_STYLE('Opaque(160,160,160)',(#27814));
#27813=FILL_AREA_STYLE_COLOUR('Steel - Satin',#27815);
#27814=FILL_AREA_STYLE_COLOUR('Opaque(160,160,160)',#27816);
#27815=COLOUR_RGB('Steel - Satin', 0.09019608, 0.27058824, 0.51372549);
#27816=COLOUR_RGB('Opaque(160,160,160)', 0.09019608, 0.27058824, 0.51372549);
ENDSEC;
END-ISO-10303-21;
